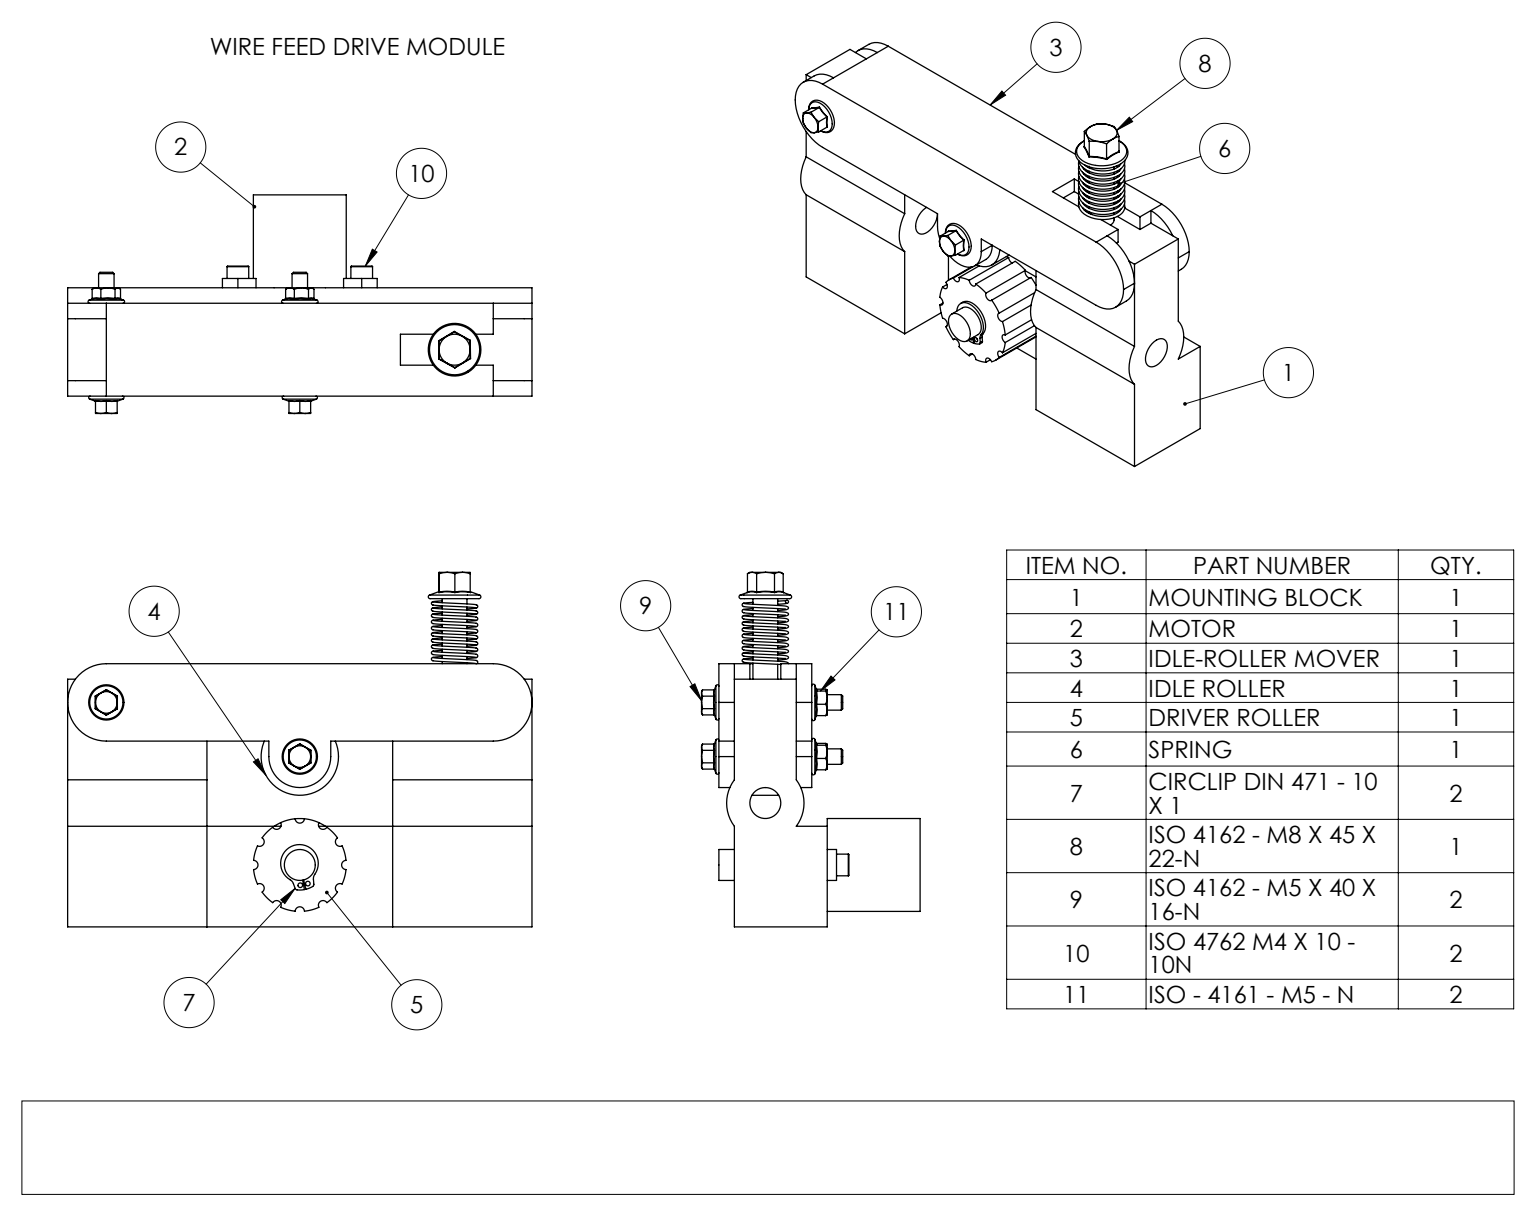
ISO-10303-21;
HEADER;
FILE_DESCRIPTION (('STEP AP214'),
    '1' );
FILE_NAME ('MAS-183',
    '2026-10-25T07:12:54',
    ( '' ),
    ( '' ),
    'SwSTEP 2.0',
    'SolidWorks 2026',
    '' );
FILE_SCHEMA (( 'AUTOMOTIVE_DESIGN' ));
ENDSEC;

DATA;
#1 = CARTESIAN_POINT ( 'NONE',  ( 44.30067958973594955, 46.10051614449766078, -1.875703265242155693 ) ) ;
#2 = CARTESIAN_POINT ( 'NONE',  ( 43.33558569842706021, 59.90051614449766504, 2.141517661632167169 ) ) ;
#3 = CARTESIAN_POINT ( 'NONE',  ( 56.81924384183011512, 48.19948385550240744, 4.924951120819313743 ) ) ;
#4 = DIRECTION ( 'NONE',  ( 0.4999999999999977796, 0.8660254037844398178, 0.000000000000000000 ) ) ;
#5 = CARTESIAN_POINT ( 'NONE',  ( 49.97728705011495265, 53.50051614449767357, 8.000000000000001776 ) ) ;
#6 =( REPRESENTATION_RELATIONSHIP ('NONE','NONE', #5328, #4503 ) REPRESENTATION_RELATIONSHIP_WITH_TRANSFORMATION ( #11054 )SHAPE_REPRESENTATION_RELATIONSHIP( ) );
#8 = EDGE_CURVE ( 'NONE', #8677, #8586, #7240, .T. ) ;
#7 = EDGE_LOOP ( 'NONE', ( #12409, #2488, #778, #882 ) ) ;
#9 = STYLED_ITEM ( 'NONE', ( #1512 ), #12751 ) ;
#10 = ORIENTED_EDGE ( 'NONE', *, *, #6895, .T. ) ;
#11 = ORIENTED_EDGE ( 'NONE', *, *, #3487, .F. ) ;
#12 = AXIS2_PLACEMENT_3D ( 'NONE', #12108, #3741, #674 ) ;
#13 = CARTESIAN_POINT ( 'NONE',  ( 62.49999999999998579, 40.00000000000001421, 0.000000000000000000 ) ) ;
#14 = SURFACE_STYLE_FILL_AREA ( #11634 ) ;
#15 = CARTESIAN_POINT ( 'NONE',  ( 2.449293598294706513E-15, -35.00000000000000000, 9.000000000000000000 ) ) ;
#16 = CARTESIAN_POINT ( 'NONE',  ( -2.100000000000000089, 2.571758278209441957E-16, -4.694516984716113228 ) ) ;
#17 = CARTESIAN_POINT ( 'NONE',  ( 44.28664221472220675, 51.09948385550240602, -1.832500667257165317 ) ) ;
#18 = CARTESIAN_POINT ( 'NONE',  ( 44.03140696652193498, 63.19948385550240744, -4.306917132069424170 ) ) ;
#19 = ADVANCED_FACE ( 'NONE', ( #12392 ), #1035, .T. ) ;
#20 = CARTESIAN_POINT ( 'NONE',  ( 47.70284917648459100, 63.60051614449766078, 6.992620115222796251 ) ) ;
#21 = AXIS2_PLACEMENT_3D ( 'NONE', #13643, #10746, #12742 ) ;
#22 = EDGE_CURVE ( 'NONE', #9726, #725, #6704, .T. ) ;
#23 = DIRECTION ( 'NONE',  ( 1.000000000000000000, 3.469446951953615668E-16, -0.000000000000000000 ) ) ;
#24 = DIRECTION ( 'NONE',  ( -1.000000000000000000, 9.251858538542972814E-17, -0.000000000000000000 ) ) ;
#25 = DIRECTION ( 'NONE',  ( -0.000000000000000000, -0.000000000000000000, 1.000000000000000000 ) ) ;
#26 = CARTESIAN_POINT ( 'NONE',  ( 57.36023556966787851, 57.00051614449766646, 0.02388180880515038476 ) ) ;
#27 = CARTESIAN_POINT ( 'NONE',  ( 55.69932041026404335, 55.89948385550241028, -1.875703265242203432 ) ) ;
#28 = FACE_OUTER_BOUND ( 'NONE', #7057, .T. ) ;
#29 = ORIENTED_EDGE ( 'NONE', *, *, #7296, .F. ) ;
#30 = CARTESIAN_POINT ( 'NONE',  ( 22.14999999999999858, -20.00000000000000000, -23.00000000000000000 ) ) ;
#31 = ORIENTED_EDGE ( 'NONE', *, *, #5701, .T. ) ;
#32 = FACE_OUTER_BOUND ( 'NONE', #8639, .T. ) ;
#33 = AXIS2_PLACEMENT_3D ( 'NONE', #4037, #13487, #9223 ) ;
#34 = PRODUCT_DEFINITION_SHAPE ( 'NONE', 'NONE',  #13671 ) ;
#35 = VECTOR ( 'NONE', #3248, 1000.000000000000000 ) ;
#36 = FACE_OUTER_BOUND ( 'NONE', #13516, .T. ) ;
#37 = DIRECTION ( 'NONE',  ( 1.000000000000000000, 0.000000000000000000, 0.000000000000000000 ) ) ;
#38 = DIRECTION ( 'NONE',  ( 0.000000000000000000, 0.000000000000000000, 1.000000000000000000 ) ) ;
#39 = CARTESIAN_POINT ( 'NONE',  ( 54.13287192849676188, 50.29948385550240175, 5.649768623646098220 ) ) ;
#40 = EDGE_CURVE ( 'NONE', #11408, #11811, #8258, .T. ) ;
#41 = CARTESIAN_POINT ( 'NONE',  ( -1.360585162435467455, 4.061296242128285883, -3.505054077164959203 ) ) ;
#42 = CARTESIAN_POINT ( 'NONE',  ( 51.97223112728249816, 54.60051614449766788, -5.992620115222793586 ) ) ;
#43 = CARTESIAN_POINT ( 'NONE',  ( 6.367873360227555679, -2.886751345948119774, 4.999999999999999112 ) ) ;
#44 = CARTESIAN_POINT ( 'NONE',  ( 49.97728705011488159, 65.49948385550240459, -7.000000000000000888 ) ) ;
#45 = CARTESIAN_POINT ( 'NONE',  ( 56.65037692655918988, 61.89948385550241028, -2.184720259617163762 ) ) ;
#46 = CARTESIAN_POINT ( 'NONE',  ( 56.65037692655918988, 57.89948385550240317, -2.184720259617163762 ) ) ;
#47 = VECTOR ( 'NONE', #619, 1000.000000000000000 ) ;
#48 = TOROIDAL_SURFACE ( 'NONE', #12842, 7.900000000000002132, 0.5999999999999979794 ) ;
#49 = VECTOR ( 'NONE', #8618, 1000.000000000000000 ) ;
#50 = ORIENTED_EDGE ( 'NONE', *, *, #11088, .F. ) ;
#51 = ORIENTED_EDGE ( 'NONE', *, *, #11790, .T. ) ;
#52 = EDGE_CURVE ( 'NONE', #12021, #8324, #11821, .T. ) ;
#53 = PLANE ( 'NONE',  #5492 ) ;
#54 = CARTESIAN_POINT ( 'NONE',  ( 3.861362476283255685, 2.629030857715988656, -3.671615880910370500 ) ) ;
#55 = CARTESIAN_POINT ( 'NONE',  ( 4.055492966679659084, -3.795017426214758682, 0.5629142681442622642 ) ) ;
#56 = VECTOR ( 'NONE', #10401, 1000.000000000000114 ) ;
#57 = CARTESIAN_POINT ( 'NONE',  ( 2.000000000000000000, 0.000000000000000000, 0.000000000000000000 ) ) ;
#58 = CARTESIAN_POINT ( 'NONE',  ( 56.66441430157296821, 48.09948385550240602, 2.141517661632100111 ) ) ;
#59 = AXIS2_PLACEMENT_3D ( 'NONE', #3052, #893, #11418 ) ;
#60 = CARTESIAN_POINT ( 'NONE',  ( 56.66441430157294690, 48.90051614449766504, -2.141517661632166281 ) ) ;
#61 = DIRECTION ( 'NONE',  ( -1.000000000000000000, 0.000000000000000000, 0.000000000000000000 ) ) ;
#62 = CARTESIAN_POINT ( 'NONE',  ( 47.42335538002188144, 62.59948385550238470, 8.007379884777233059 ) ) ;
#63 =( LENGTH_UNIT ( ) NAMED_UNIT ( * ) SI_UNIT ( .MILLI., .METRE. ) );
#64 = CARTESIAN_POINT ( 'NONE',  ( 56.79116909180255135, 53.79948385550241596, -4.963592699179005585 ) ) ;
#65 = VERTEX_POINT ( 'NONE', #4105 ) ;
#66 = CIRCLE ( 'NONE', #7586, 1.500000000000001110 ) ;
#67 = EDGE_LOOP ( 'NONE', ( #6510, #1768, #3467, #950 ) ) ;
#68 = LINE ( 'NONE', #4288, #2309 ) ;
#69 = CARTESIAN_POINT ( 'NONE',  ( 6.207671477327291853, -3.321994320370684317, 4.246137054662720622 ) ) ;
#70=STYLED_ITEM('',(#13712),#1029);
#71 = FACE_OUTER_BOUND ( 'NONE', #6413, .T. ) ;
#72 = CARTESIAN_POINT ( 'NONE',  ( 55.08986747509849380, 47.20051614449766220, 3.727524721679155384 ) ) ;
#73 = CARTESIAN_POINT ( 'NONE',  ( 52.25172492374528588, 57.40051614449765793, 7.007379884777204637 ) ) ;
#74 = CARTESIAN_POINT ( 'NONE',  ( 52.57664461997811856, 45.59948385550240602, -8.007379884777229506 ) ) ;
#75 = CARTESIAN_POINT ( 'NONE',  ( 4.052424581287595196, 3.786734753434853662, 0.5771415817955924954 ) ) ;
#76 = CARTESIAN_POINT ( 'NONE',  ( 58.41169779390614281, 55.00051614449766646, 0.02388180880515032231 ) ) ;
#77 = ORIENTED_EDGE ( 'NONE', *, *, #7381, .F. ) ;
#78 = ORIENTED_EDGE ( 'NONE', *, *, #4870, .T. ) ;
#79 = ORIENTED_EDGE ( 'NONE', *, *, #8111, .F. ) ;
#80 = CYLINDRICAL_SURFACE ( 'NONE', #13518, 1.500000000000001332 ) ;
#81 = EDGE_CURVE ( 'NONE', #6144, #12887, #9290, .T. ) ;
#83 = CIRCLE ( 'NONE', #7166, 4.999999999999999112 ) ;
#82 = PLANE ( 'NONE',  #5621 ) ;
#84 = CARTESIAN_POINT ( 'NONE',  ( 5.599999999999999645, 4.041451884327382338, 0.000000000000000000 ) ) ;
#85 = DIRECTION ( 'NONE',  ( 1.000000000000000000, -0.000000000000000000, 0.000000000000000000 ) ) ;
#86 = CARTESIAN_POINT ( 'NONE',  ( 48.02776887271745210, 49.39948385550241028, -5.992620115222778487 ) ) ;
#87 = CARTESIAN_POINT ( 'NONE',  ( 4.050880675075949178, 1.379097446046194220, 3.567934390854430760 ) ) ;
#88 = CARTESIAN_POINT ( 'NONE',  ( 54.72065718078918906, 48.70051614449766930, -6.458785618021089192 ) ) ;
#89 = CARTESIAN_POINT ( 'NONE',  ( 4.000000000000000888, 1.539600717838996990, -3.300726591567079815 ) ) ;
#90 = CARTESIAN_POINT ( 'NONE',  ( 0.08165819712376973238, 4.939961795957293234, 1.443735181952769064 ) ) ;
#91 = CARTESIAN_POINT ( 'NONE',  ( 47.74827507625469281, 54.40051614449766504, -7.007379884777203749 ) ) ;
#92 = CARTESIAN_POINT ( 'NONE',  ( 50.02271294988511841, 56.49948385550240459, 6.000000000000000888 ) ) ;
#93 = CARTESIAN_POINT ( 'NONE',  ( 2.000000000000000000, -6.429618962271402616, -1.000000000000000000 ) ) ;
#94 = ADVANCED_FACE ( 'NONE', ( #8455 ), #6331, .F. ) ;
#95 = CIRCLE ( 'NONE', #11121, 2.649999999999988365 ) ;
#96 = ORIENTED_EDGE ( 'NONE', *, *, #7070, .F. ) ;
#97 = ADVANCED_FACE ( 'NONE', ( #1883, #8329, #2085 ), #7362, .T. ) ;
#98 = DIRECTION ( 'NONE',  ( 0.000000000000000000, -1.000000000000000000, 0.000000000000000000 ) ) ;
#99 = EDGE_CURVE ( 'NONE', #9288, #2470, #13475, .T. ) ;
#100 = AXIS2_PLACEMENT_3D ( 'NONE', #7790, #12001, #438 ) ;
#101 = ORIENTED_EDGE ( 'NONE', *, *, #5437, .F. ) ;
#102 = DIRECTION ( 'NONE',  ( 1.000000000000000000, 0.000000000000000000, 0.000000000000000000 ) ) ;
#103 = EDGE_CURVE ( 'NONE', #12840, #3906, #7426, .T. ) ;
#104 = DIRECTION ( 'NONE',  ( -9.710251638871371392E-17, -5.969973981896233748E-17, -1.000000000000000000 ) ) ;
#105 = CARTESIAN_POINT ( 'NONE',  ( 4.093692494532774617, 2.021783646005766322, -3.501831996793843160 ) ) ;
#106 = SURFACE_STYLE_USAGE ( .BOTH. , #7508 ) ;
#107 = CARTESIAN_POINT ( 'NONE',  ( 54.13287192849676188, 52.29948385550240886, 5.649768623646098220 ) ) ;
#108 = AXIS2_PLACEMENT_3D ( 'NONE', #135, #10772, #2266 ) ;
#109 = CARTESIAN_POINT ( 'NONE',  ( 53.50833635130544508, 51.30051614449765651, 4.867452303228181343 ) ) ;
#110 = CARTESIAN_POINT ( 'NONE',  ( 2.385244779468109755E-15, -20.00000000000000000, -9.999999999999994671 ) ) ;
#111 = LINE ( 'NONE', #5314, #1494 ) ;
#112 = CARTESIAN_POINT ( 'NONE',  ( 6.466260427357665819, -5.808561367196025671, 1.503437176544561004E-15 ) ) ;
#113 = CARTESIAN_POINT ( 'NONE',  ( 47.74827507625478518, 60.59948385550239891, 7.007379884777227730 ) ) ;
#114 = CARTESIAN_POINT ( 'NONE',  ( -0.2500000000000000000, -8.096141056083446585, -1.000000000000000000 ) ) ;
#115 = ORIENTED_EDGE ( 'NONE', *, *, #9892, .T. ) ;
#116 = EDGE_LOOP ( 'NONE', ( #1810, #12426, #10336 ) ) ;
#117 = AXIS2_PLACEMENT_3D ( 'NONE', #12874, #6605, #168 ) ;
#118 = ORIENTED_EDGE ( 'NONE', *, *, #4262, .T. ) ;
#119 = CARTESIAN_POINT ( 'NONE',  ( -1.287237434361707233, -3.875615274277397937, -3.430618716626816500 ) ) ;
#120 = ADVANCED_FACE ( 'NONE', ( #5352 ), #80, .F. ) ;
#121 = B_SPLINE_CURVE_WITH_KNOTS ( 'NONE', 3,
 ( #11045, #8921, #1705, #7048, #10078, #9050 ),
 .UNSPECIFIED., .F., .F.,
 ( 4, 2, 4 ),
 ( 0.000000000000000000, 0.002086519881787260184, 0.004173039763574520368 ),
 .UNSPECIFIED. ) ;
#122 = CARTESIAN_POINT ( 'NONE',  ( 0.000000000000000000, 0.000000000000000000, 0.000000000000000000 ) ) ;
#123 = CARTESIAN_POINT ( 'NONE',  ( -3.355112389629170799, 2.681727112203152963, -0.2256878752776689534 ) ) ;
#124 = CARTESIAN_POINT ( 'NONE',  ( 4.024499207728657879, 2.323545700935571556, -3.572172305156506411 ) ) ;
#125 = CARTESIAN_POINT ( 'NONE',  ( 56.65037692655918988, 49.89948385550240317, -2.184720259617163762 ) ) ;
#126 = CARTESIAN_POINT ( 'NONE',  ( 56.65037692655921120, 45.10051614449766078, 2.184720259617097593 ) ) ;
#127 = DIRECTION ( 'NONE',  ( 0.000000000000000000, 0.000000000000000000, 1.000000000000000000 ) ) ;
#128 = CARTESIAN_POINT ( 'NONE',  ( 50.02271294988512551, 48.49948385550240459, 7.000000000000000888 ) ) ;
#129 = CYLINDRICAL_SURFACE ( 'NONE', #612, 2.500000000000000444 ) ;
#130 = CARTESIAN_POINT ( 'NONE',  ( 56.81924384183011512, 54.19948385550241454, 4.924951120819313743 ) ) ;
#131 = ORIENTED_EDGE ( 'NONE', *, *, #11542, .F. ) ;
#132 = EDGE_CURVE ( 'NONE', #594, #13026, #10926, .T. ) ;
#133 = EDGE_LOOP ( 'NONE', ( #295, #3127 ) ) ;
#134 = EDGE_CURVE ( 'NONE', #822, #8082, #1591, .T. ) ;
#135 = CARTESIAN_POINT ( 'NONE',  ( 1.267864665261691752E-11, -20.00000000000000000, 9.999999999999998224 ) ) ;
#136 = AXIS2_PLACEMENT_3D ( 'NONE', #12197, #10046, #9019 ) ;
#137 = CARTESIAN_POINT ( 'NONE',  ( 50.00000000000000000, 40.00000000000000000, 0.000000000000000000 ) ) ;
#138 = CARTESIAN_POINT ( 'NONE',  ( 46.45491332379576477, 49.70051614449766220, 4.840751629271188961 ) ) ;
#139 = CARTESIAN_POINT ( 'NONE',  ( 47.74827507625470702, 60.40051614449766504, -7.007379884777204637 ) ) ;
#140 = CARTESIAN_POINT ( 'NONE',  ( 47.37792948025170858, 63.60051614449764656, 7.992620115222797139 ) ) ;
#141 = CARTESIAN_POINT ( 'NONE',  ( -75.00000000000001421, -5.000000000000025757, 6.123233995736775157E-16 ) ) ;
#142 = B_SPLINE_CURVE_WITH_KNOTS ( 'NONE', 3,
 ( #2843, #11275, #8032, #7064, #8173 ),
 .UNSPECIFIED., .F., .F.,
 ( 4, 1, 4 ),
 ( 0.000000000000000000, 0.002020725942163692675, 0.004041451884327385349 ),
 .UNSPECIFIED. ) ;
#143 = CARTESIAN_POINT ( 'NONE',  ( 47.37792948025170858, 53.60051614449765367, 7.992620115222797139 ) ) ;
#144 = B_SPLINE_CURVE_WITH_KNOTS ( 'NONE', 3,
 ( #13141, #2570, #7772, #10101, #12115, #12051, #4654, #11983, #6798, #4863, #3822, #8039 ),
 .UNSPECIFIED., .F., .F.,
 ( 4, 2, 2, 2, 2, 4 ),
 ( 0.01755862241325779893, 0.01812962329865995884, 0.01870062418406211874, 0.01984262595486643854, 0.02098462772567075835, 0.02212662949647507815 ),
 .UNSPECIFIED. ) ;
#145 = PRODUCT_DEFINITION_SHAPE ( 'NONE', 'NONE',  #13669 ) ;
#146 = ORIENTED_EDGE ( 'NONE', *, *, #5916, .F. ) ;
#147 = CONICAL_SURFACE ( 'NONE', #11179, 8.105212085995399107, 1.221730476396037490 ) ;
#148 = ORIENTED_EDGE ( 'NONE', *, *, #10663, .F. ) ;
#149 = ORIENTED_EDGE ( 'NONE', *, *, #1777, .T. ) ;
#150 = ORIENTED_EDGE ( 'NONE', *, *, #2542, .F. ) ;
#151 = DIRECTION ( 'NONE',  ( -0.5000000000000041078, 0.8660254037844362651, 0.000000000000000000 ) ) ;
#152 = FACE_OUTER_BOUND ( 'NONE', #7758, .T. ) ;
#153 = FACE_OUTER_BOUND ( 'NONE', #3940, .T. ) ;
#154 = FACE_OUTER_BOUND ( 'NONE', #10455, .T. ) ;
#155 = CARTESIAN_POINT ( 'NONE',  ( 55.71335778527780747, 50.09948385550240602, 1.832500667257165983 ) ) ;
#156 = CARTESIAN_POINT ( 'NONE',  ( 47.74827507625477807, 64.59948385550239891, 7.007379884777229506 ) ) ;
#157 = ADVANCED_FACE ( 'NONE', ( #8524 ), #11972, .T. ) ;
#158 = CARTESIAN_POINT ( 'NONE',  ( 45.90387839640208512, 64.30051614449766362, -5.676469297603124353 ) ) ;
#159 = DIRECTION ( 'NONE',  ( -1.000000000000000000, 0.000000000000000000, 0.000000000000000000 ) ) ;
#160 = CARTESIAN_POINT ( 'NONE',  ( 4.000000000000003553, 4.286263797015736595E-16, -3.500000000000000000 ) ) ;
#161 = CARTESIAN_POINT ( 'NONE',  ( 45.90387839640208512, 54.30051614449765651, -5.676469297603124353 ) ) ;
#162 = CARTESIAN_POINT ( 'NONE',  ( 55.11794222512601493, 60.19948385550240744, 3.688883143319541702 ) ) ;
#163 = ADVANCED_FACE ( 'NONE', ( #12857 ), #1236, .F. ) ;
#164 = ORIENTED_EDGE ( 'NONE', *, *, #12600, .T. ) ;
#165 = CARTESIAN_POINT ( 'NONE',  ( -9.999999999999996447, 0.000000000000000000, 9.999999999999998224 ) ) ;
#166 = ORIENTED_EDGE ( 'NONE', *, *, #5950, .F. ) ;
#167 = CARTESIAN_POINT ( 'NONE',  ( -75.00000000000001421, -2.602085213965211904E-14, 0.000000000000000000 ) ) ;
#168 = DIRECTION ( 'NONE',  ( 0.000000000000000000, 0.000000000000000000, 1.000000000000000000 ) ) ;
#169 = CARTESIAN_POINT ( 'NONE',  ( -4.000000000000000000, -0.7890432684750890990, -0.04868663549882315533 ) ) ;
#170 = CARTESIAN_POINT ( 'NONE',  ( 45.86712807150323812, 53.29948385550240886, -5.649768623646098220 ) ) ;
#171 = PLANE ( 'NONE',  #421 ) ;
#172 = CARTESIAN_POINT ( 'NONE',  ( 48.02776887271750184, 51.60051614449766788, 5.992620115222795363 ) ) ;
#173 = DIRECTION ( 'NONE',  ( 1.000000000000000000, 0.000000000000000000, 0.000000000000000000 ) ) ;
#174 = FACE_OUTER_BOUND ( 'NONE', #12287, .T. ) ;
#175 = CARTESIAN_POINT ( 'NONE',  ( 6.527192678185836705, -5.883244248022288403, -1.193258867985458992E-13 ) ) ;
#176 = CARTESIAN_POINT ( 'NONE',  ( 55.94051828345050836, 57.79948385550238754, -4.345558710429104465 ) ) ;
#177 = FACE_OUTER_BOUND ( 'NONE', #6171, .T. ) ;
#178 = VERTEX_POINT ( 'NONE', #7689 ) ;
#179 = ORIENTED_EDGE ( 'NONE', *, *, #103, .F. ) ;
#180 = SHAPE_REPRESENTATION ( 'hex flange nut gradea_iso_ISO - 4161 - M5 - N', ( #430 ), #9487 ) ;
#181 = ORIENTED_EDGE ( 'NONE', *, *, #4567, .T. ) ;
#182 = FACE_OUTER_BOUND ( 'NONE', #2923, .T. ) ;
#183 = FACE_OUTER_BOUND ( 'NONE', #3328, .T. ) ;
#184 = CARTESIAN_POINT ( 'NONE',  ( 4.033901012035946643, -3.740908793664254883, 0.5205559028926849408 ) ) ;
#185 =( NAMED_UNIT ( * ) SI_UNIT ( $, .STERADIAN. ) SOLID_ANGLE_UNIT ( ) );
#186 = FACE_OUTER_BOUND ( 'NONE', #2806, .T. ) ;
#187 = CARTESIAN_POINT ( 'NONE',  ( 45.86712807150323812, 51.29948385550240175, -5.649768623646098220 ) ) ;
#188 = CARTESIAN_POINT ( 'NONE',  ( 47.74827507625469281, 56.40051614449766504, -7.007379884777203749 ) ) ;
#189 = CIRCLE ( 'NONE', #9683, 1.610000000000000098 ) ;
#190 = FACE_OUTER_BOUND ( 'NONE', #6460, .T. ) ;
#191 = CARTESIAN_POINT ( 'NONE',  ( 54.72065718078924590, 64.29948385550240175, 6.458785618021043895 ) ) ;
#192 = ADVANCED_FACE ( 'NONE', ( #1373 ), #9888, .F. ) ;
#193 = CYLINDRICAL_SURFACE ( 'NONE', #11066, 15.00000000000000000 ) ;
#194 = EDGE_CURVE ( 'NONE', #11144, #6641, #2280, .T. ) ;
#195 = B_SPLINE_CURVE_WITH_KNOTS ( 'NONE', 3,
 ( #11262, #10080, #4985, #5816, #13250 ),
 .UNSPECIFIED., .F., .F.,
 ( 4, 1, 4 ),
 ( 0.000000000000000000, 0.002886751345948130286, 0.005773502691896260572 ),
 .UNSPECIFIED. ) ;
#196 = CARTESIAN_POINT ( 'NONE',  ( 45.27934281921075410, 57.29948385550240175, -6.458785618021043895 ) ) ;
#197 = EDGE_CURVE ( 'NONE', #1117, #3434, #12820, .T. ) ;
#198 = ORIENTED_EDGE ( 'NONE', *, *, #8722, .T. ) ;
#199 = ORIENTED_EDGE ( 'NONE', *, *, #13522, .F. ) ;
#200 = CARTESIAN_POINT ( 'NONE',  ( 32.49999999999998579, 40.00000000000001421, -4.999999999999996447 ) ) ;
#201 = CIRCLE ( 'NONE', #9264, 1.500000000000000222 ) ;
#202 = CARTESIAN_POINT ( 'NONE',  ( -14.99999999999999822, -19.99999999999999645, -23.00000000000000000 ) ) ;
#203 = CARTESIAN_POINT ( 'NONE',  ( 43.69122665457040000, 56.00051614449765935, -0.02388180880515696977 ) ) ;
#204 = CARTESIAN_POINT ( 'NONE',  ( 8.673617379884035472E-16, 4.618802153517012954, 0.000000000000000000 ) ) ;
#205 = PRESENTATION_LAYER_ASSIGNMENT (  '', '', ( #8165 ) ) ;
#206 = CARTESIAN_POINT ( 'NONE',  ( 54.68390685589033495, 45.69948385550240033, -6.485486291978119766 ) ) ;
#207 = VECTOR ( 'NONE', #526, 1000.000000000000000 ) ;
#208 = CARTESIAN_POINT ( 'NONE',  ( 2.449293598294706513E-15, -20.00000000000000000, -9.000000000000000000 ) ) ;
#209 = CARTESIAN_POINT ( 'NONE',  ( 45.27934281921082516, 53.70051614449766220, 6.458785618021089192 ) ) ;
#210 = ORIENTED_EDGE ( 'NONE', *, *, #1266, .T. ) ;
#211 = ORIENTED_EDGE ( 'NONE', *, *, #8650, .F. ) ;
#212 = ORIENTED_EDGE ( 'NONE', *, *, #12682, .T. ) ;
#213 = ORIENTED_EDGE ( 'NONE', *, *, #10321, .T. ) ;
#214 = AXIS2_PLACEMENT_3D ( 'NONE', #5780, #4595, #6805 ) ;
#215 = DIRECTION ( 'NONE',  ( 0.000000000000000000, 0.000000000000000000, 1.000000000000000000 ) ) ;
#216 = EDGE_CURVE ( 'NONE', #11745, #13576, #7487, .T. ) ;
#218 = CIRCLE ( 'NONE', #6639, 5.000000000000000000 ) ;
#217 = DIRECTION ( 'NONE',  ( -0.000000000000000000, -0.000000000000000000, -1.000000000000000000 ) ) ;
#219 = FACE_BOUND ( 'NONE', #1402, .T. ) ;
#220 = CARTESIAN_POINT ( 'NONE',  ( -74.99999999999997158, 20.00000000000001421, 15.00000000000000000 ) ) ;
#221 = CYLINDRICAL_SURFACE ( 'NONE', #6994, 2.000000000000000888 ) ;
#222 = CARTESIAN_POINT ( 'NONE',  ( 51.97223112728254790, 50.39948385550241738, 5.992620115222778487 ) ) ;
#223 = CARTESIAN_POINT ( 'NONE',  ( 43.33558569842703179, 63.09948385550240602, -2.141517661632099223 ) ) ;
#224 = CARTESIAN_POINT ( 'NONE',  ( 41.58830220609386430, 48.00051614449766646, -0.02388180880514929535 ) ) ;
#225 = CARTESIAN_POINT ( 'NONE',  ( -0.1481481481481481122, -4.797713218419819903, -1.000000000000000000 ) ) ;
#226 = CARTESIAN_POINT ( 'NONE',  ( -4.000000000000000000, -2.309401076758512694, -5.000000000000000000 ) ) ;
#227 = EDGE_CURVE ( 'NONE', #4104, #6571, #11764, .T. ) ;
#228 = CARTESIAN_POINT ( 'NONE',  ( 56.65037692655921120, 57.10051614449766078, 2.184720259617097593 ) ) ;
#229 =( GEOMETRIC_REPRESENTATION_CONTEXT ( 3 ) GLOBAL_UNCERTAINTY_ASSIGNED_CONTEXT ( ( #8327 ) ) GLOBAL_UNIT_ASSIGNED_CONTEXT ( ( #1931, #1865, #3739 ) ) REPRESENTATION_CONTEXT ( 'NONE', 'WORKASPACE' ) );
#230 = CARTESIAN_POINT ( 'NONE',  ( 55.71335778527780747, 58.09948385550241312, 1.832500667257165983 ) ) ;
#231 = VECTOR ( 'NONE', #11750, 1000.000000000000000 ) ;
#232 = ORIENTED_EDGE ( 'NONE', *, *, #13179, .F. ) ;
#233 = PLANE ( 'NONE',  #5515 ) ;
#234 = ORIENTED_EDGE ( 'NONE', *, *, #2081, .F. ) ;
#235 = CARTESIAN_POINT ( 'NONE',  ( 6.527192678185834041, 2.941622124011172623, 5.095038975455953079 ) ) ;
#236 = FACE_OUTER_BOUND ( 'NONE', #5614, .T. ) ;
#237 = CARTESIAN_POINT ( 'NONE',  ( 4.050823680195223098, 2.400527758044901372, 2.978030508226146900 ) ) ;
#238 = CARTESIAN_POINT ( 'NONE',  ( 45.90387839640214196, 48.69948385550240744, 5.676469297603166098 ) ) ;
#239 = CARTESIAN_POINT ( 'NONE',  ( 2.449293598294706513E-15, -20.00000000000000000, 9.000000000000000000 ) ) ;
#240 = CARTESIAN_POINT ( 'NONE',  ( 43.69122665457040000, 60.00051614449765935, -0.02388180880515696977 ) ) ;
#241 = CARTESIAN_POINT ( 'NONE',  ( -30.00000000000000000, 7.499999999999991118, 10.00000000000000000 ) ) ;
#242 = DIRECTION ( 'NONE',  ( 1.000000000000000000, 0.000000000000000000, 0.000000000000000000 ) ) ;
#243 = CARTESIAN_POINT ( 'NONE',  ( 52.29715082351547295, 60.39948385550239607, 6.992620115222774047 ) ) ;
#244 = DIRECTION ( 'NONE',  ( 0.000000000000000000, -0.000000000000000000, 1.000000000000000000 ) ) ;
#245 = VERTEX_POINT ( 'NONE', #4504 ) ;
#246 = VECTOR ( 'NONE', #11169, 1000.000000000000000 ) ;
#247 = ORIENTED_EDGE ( 'NONE', *, *, #4058, .T. ) ;
#248 = CARTESIAN_POINT ( 'NONE',  ( 0.1410422978106145031, -4.700232962125109104, -3.687027686973628704 ) ) ;
#249 = DIRECTION ( 'NONE',  ( 0.000000000000000000, 0.000000000000000000, 1.000000000000000000 ) ) ;
#250 = DIRECTION ( 'NONE',  ( -0.7581610723493046322, -0.6520673188974834833, 1.125475972357111981E-16 ) ) ;
#251 = CARTESIAN_POINT ( 'NONE',  ( 20.00000000000000000, -20.00000000000000000, -12.00000000000000000 ) ) ;
#252 = FACE_BOUND ( 'NONE', #2068, .T. ) ;
#253 = CARTESIAN_POINT ( 'NONE',  ( 43.34962307344081012, 54.89948385550240317, 2.184720259617164650 ) ) ;
#254 = CARTESIAN_POINT ( 'NONE',  ( 56.65037692655921120, 55.10051614449766078, 2.184720259617097593 ) ) ;
#255 = CARTESIAN_POINT ( 'NONE',  ( 75.00000000000001421, 2.602085213965211904E-14, 0.000000000000000000 ) ) ;
#256 = AXIS2_PLACEMENT_3D ( 'NONE', #2457, #12077, #2596 ) ;
#257 = CARTESIAN_POINT ( 'NONE',  ( 43.33558569842703179, 49.09948385550240602, -2.141517661632099223 ) ) ;
#258 =( BOUNDED_SURFACE ( )  B_SPLINE_SURFACE ( 3, 2, ( 
 ( #4456, #8885, #3626 ),
 ( #7848, #4733, #425 ),
 ( #12875, #2579, #6804 ),
 ( #11009, #4594, #5571 ),
 ( #1531, #5776, #3689 ),
 ( #9780, #6677, #7912 ) ),
 .UNSPECIFIED., .F., .F., .F. ) 
 B_SPLINE_SURFACE_WITH_KNOTS ( ( 4, 2, 4 ),
 ( 3, 3 ),
 ( 0.01651999345535506980, 0.01858032176739836394, 0.02064065007944165808 ),
 ( 0.000000000000000000, 1.000000000000000000 ),
 .UNSPECIFIED. ) 
 GEOMETRIC_REPRESENTATION_ITEM ( )  RATIONAL_B_SPLINE_SURFACE ( (
 ( 1.000000000000000000, 0.8047781103519393575, 1.000000000000000000),
 ( 1.000000000000000000, 0.8123785825603968558, 1.000000000000000000),
 ( 1.000000000000000000, 0.8190671539788806355, 1.000000000000000000),
 ( 1.000000000000000000, 0.8192352254834333047, 1.000000000000000000),
 ( 1.000000000000000000, 0.8126129677212012847, 1.000000000000000000),
 ( 1.000000000000000000, 0.8047712537969730073, 1.000000000000000000) ) ) 
 REPRESENTATION_ITEM ( '' )  SURFACE ( )  );
#259 = CARTESIAN_POINT ( 'NONE',  ( 47.42335538002188144, 62.59948385550238470, 8.007379884777233059 ) ) ;
#260 = EDGE_CURVE ( 'NONE', #13554, #4523, #9345, .T. ) ;
#261 = ORIENTED_EDGE ( 'NONE', *, *, #227, .F. ) ;
#262 = AXIS2_PLACEMENT_3D ( 'NONE', #4018, #5829, #10026 ) ;
#263 = ORIENTED_EDGE ( 'NONE', *, *, #4115, .F. ) ;
#264 = ADVANCED_FACE ( 'NONE', ( #3266 ), #5618, .F. ) ;
#265 = CARTESIAN_POINT ( 'NONE',  ( 2.449293598294706513E-15, -20.00000000000000000, 9.000000000000000000 ) ) ;
#266 = ADVANCED_FACE ( 'NONE', ( #8732 ), #10661, .F. ) ;
#267 = EDGE_CURVE ( 'NONE', #10003, #9221, #8792, .T. ) ;
#268 = DIRECTION ( 'NONE',  ( 0.3420201433256622736, 0.000000000000000000, -0.9396926207859106484 ) ) ;
#269 = CARTESIAN_POINT ( 'NONE',  ( 46.45491332379576477, 51.70051614449765509, 4.840751629271188961 ) ) ;
#270 = CARTESIAN_POINT ( 'NONE',  ( -3.333333333333335258, 2.694301256218251783, -3.300726591567079815 ) ) ;
#271 = CARTESIAN_POINT ( 'NONE',  ( 52.57664461997811856, 51.59948385550240602, -8.007379884777229506 ) ) ;
#272 = EDGE_CURVE ( 'NONE', #12293, #940, #9194, .T. ) ;
#273 = CARTESIAN_POINT ( 'NONE',  ( 55.96859303347804371, 56.19948385550241454, 4.306917132069425946 ) ) ;
#274 = CARTESIAN_POINT ( 'NONE',  ( 3.972066048304770725, 3.435565134476467275, 1.180968096049824556 ) ) ;
#275 = CARTESIAN_POINT ( 'NONE',  ( 47.42335538002180328, 58.40051614449765793, -8.007379884777206414 ) ) ;
#276 = AXIS2_PLACEMENT_3D ( 'NONE', #9355, #962, #6117 ) ;
#277 = ORIENTED_EDGE ( 'NONE', *, *, #8722, .F. ) ;
#278 = VERTEX_POINT ( 'NONE', #10857 ) ;
#279 = ORIENTED_EDGE ( 'NONE', *, *, #2210, .T. ) ;
#280 = ORIENTED_EDGE ( 'NONE', *, *, #5001, .F. ) ;
#281 = EDGE_CURVE ( 'NONE', #5149, #3301, #7761, .T. ) ;
#282 = CARTESIAN_POINT ( 'NONE',  ( -3.679171394226034675, -2.494631558665844739, -0.3503314178412558211 ) ) ;
#283 = CYLINDRICAL_SURFACE ( 'NONE', #7915, 5.000000000000000888 ) ;
#284 = EDGE_CURVE ( 'NONE', #3263, #6584, #5155, .T. ) ;
#285 = CARTESIAN_POINT ( 'NONE',  ( 0.4465819873852002742, 2.886751345948125547, 4.999999999999999112 ) ) ;
#286 = CARTESIAN_POINT ( 'NONE',  ( 1.655952806101427033, -3.662737355149048302, -1.182683869819604841E-14 ) ) ;
#287 = CARTESIAN_POINT ( 'NONE',  ( 50.02271294988511841, 54.49948385550240459, 6.000000000000000888 ) ) ;
#288 = CARTESIAN_POINT ( 'NONE',  ( 44.03140696652198471, 47.80051614449764941, 4.306917132069485454 ) ) ;
#289 = CARTESIAN_POINT ( 'NONE',  ( 52.25172492374527877, 63.40051614449765793, 7.007379884777203749 ) ) ;
#290 = DIRECTION ( 'NONE',  ( 1.000000000000000000, 0.000000000000000000, 0.000000000000000000 ) ) ;
#291 = DIRECTION ( 'NONE',  ( 0.000000000000000000, -1.000000000000000000, 0.000000000000000000 ) ) ;
#292 = CARTESIAN_POINT ( 'NONE',  ( 47.70284917648459100, 59.60051614449765367, 6.992620115222796251 ) ) ;
#293 = ORIENTED_EDGE ( 'NONE', *, *, #1456, .F. ) ;
#294 = CARTESIAN_POINT ( 'NONE',  ( 20.00000000000000000, -20.00000000000000000, -23.00000000000000000 ) ) ;
#295 = ORIENTED_EDGE ( 'NONE', *, *, #8457, .F. ) ;
#296 = CARTESIAN_POINT ( 'NONE',  ( 0.000000000000000000, 0.000000000000000000, 0.000000000000000000 ) ) ;
#297 = ADVANCED_FACE ( 'NONE', ( #10786 ), #7829, .T. ) ;
#298 = DIRECTION ( 'NONE',  ( 1.000000000000000000, 0.000000000000000000, 0.000000000000000000 ) ) ;
#299 = DIRECTION ( 'NONE',  ( -0.000000000000000000, -0.000000000000000000, -1.000000000000000000 ) ) ;
#300 = CARTESIAN_POINT ( 'NONE',  ( 55.94051828345050836, 55.79948385550238044, -4.345558710429104465 ) ) ;
#301 = CARTESIAN_POINT ( 'NONE',  ( 2.805705207896068476, -3.226868319750173075, -3.503898532754370354 ) ) ;
#302 = CARTESIAN_POINT ( 'NONE',  ( 48.07319477248762496, 60.40051614449765793, -6.007379884777208190 ) ) ;
#303 = AXIS2_PLACEMENT_3D ( 'NONE', #3624, #7847, #12122 ) ;
#304 = CARTESIAN_POINT ( 'NONE',  ( 9.999999999999994671, 20.00000000000001421, 15.00000000000000000 ) ) ;
#305 = DIRECTION ( 'NONE',  ( 0.000000000000000000, 0.000000000000000000, -1.000000000000000000 ) ) ;
#306 = FILL_AREA_STYLE ('',( #2314 ) ) ;
#307 = CARTESIAN_POINT ( 'NONE',  ( 56.65037692655918988, 63.89948385550239607, -2.184720259617163762 ) ) ;
#308 = FACE_OUTER_BOUND ( 'NONE', #7358, .T. ) ;
#309 = ORIENTED_EDGE ( 'NONE', *, *, #197, .T. ) ;
#310 = CIRCLE ( 'NONE', #5415, 1.499999999999999778 ) ;
#311 = ORIENTED_EDGE ( 'NONE', *, *, #8812, .T. ) ;
#312 = AXIS2_PLACEMENT_3D ( 'NONE', #6238, #11325, #3101 ) ;
#313 = ORIENTED_EDGE ( 'NONE', *, *, #6610, .T. ) ;
#314 = DIRECTION ( 'NONE',  ( -0.000000000000000000, -0.000000000000000000, -1.000000000000000000 ) ) ;
#315 = CIRCLE ( 'NONE', #7843, 5.371010071662833063 ) ;
#316 = DIRECTION ( 'NONE',  ( -0.000000000000000000, 1.000000000000000000, 1.224646799147353207E-16 ) ) ;
#317 = DIRECTION ( 'NONE',  ( -0.000000000000000000, -0.000000000000000000, 1.000000000000000000 ) ) ;
#318 =( NAMED_UNIT ( * ) PLANE_ANGLE_UNIT ( ) SI_UNIT ( $, .RADIAN. ) );
#319 = CARTESIAN_POINT ( 'NONE',  ( -9.999999999999994671, 20.00000000000001421, -9.999999999999998224 ) ) ;
#320 = FACE_BOUND ( 'NONE', #11284, .T. ) ;
#321 = CARTESIAN_POINT ( 'NONE',  ( 50.02271294988512551, 54.49948385550240459, 7.000000000000000888 ) ) ;
#322 = TOROIDAL_SURFACE ( 'NONE', #9170, 5.384454397937118664, 0.5155456020628804703 ) ;
#323 = CARTESIAN_POINT ( 'NONE',  ( 56.66441430157294690, 54.90051614449765793, -2.141517661632166281 ) ) ;
#324 = DIRECTION ( 'NONE',  ( 0.000000000000000000, 0.000000000000000000, 1.000000000000000000 ) ) ;
#325 = EDGE_CURVE ( 'NONE', #12408, #8324, #8870, .T. ) ;
#326 = CARTESIAN_POINT ( 'NONE',  ( 45.90387839640214196, 54.69948385550240744, 5.676469297603166098 ) ) ;
#327 = CARTESIAN_POINT ( 'NONE',  ( 55.94051828345050836, 49.79948385550240175, -4.345558710429104465 ) ) ;
#328 = CIRCLE ( 'NONE', #10491, 0.7500000000000000000 ) ;
#329 = CARTESIAN_POINT ( 'NONE',  ( 50.02271294988513972, 64.49948385550239038, 8.000000000000001776 ) ) ;
#330 = ORIENTED_EDGE ( 'NONE', *, *, #7102, .T. ) ;
#331 = VERTEX_POINT ( 'NONE', #13575 ) ;
#332 = ORIENTED_EDGE ( 'NONE', *, *, #7882, .F. ) ;
#333 = LINE ( 'NONE', #7675, #5864 ) ;
#334 = AXIS2_PLACEMENT_3D ( 'NONE', #11503, #2020, #12598 ) ;
#335 = CARTESIAN_POINT ( 'NONE',  ( -11.49038105676659249, -12.50000000000003020, -9.000000000000000000 ) ) ;
#336 = CARTESIAN_POINT ( 'NONE',  ( 48.07319477248762496, 54.40051614449765793, -6.007379884777208190 ) ) ;
#337 = CARTESIAN_POINT ( 'NONE',  ( 47.74827507625470702, 64.40051614449765793, -7.007379884777204637 ) ) ;
#338 = CARTESIAN_POINT ( 'NONE',  ( 56.79116909180255135, 49.79948385550240175, -4.963592699179005585 ) ) ;
#339 = CARTESIAN_POINT ( 'NONE',  ( 43.33558569842703179, 59.09948385550240602, -2.141517661632099223 ) ) ;
#340 = CARTESIAN_POINT ( 'NONE',  ( 2.000000000000000000, 1.773042676681340524, -2.059984127722458425E-15 ) ) ;
#341 = EDGE_CURVE ( 'NONE', #7290, #12675, #5666, .T. ) ;
#342 = CARTESIAN_POINT ( 'NONE',  ( 47.42335538002180328, 60.40051614449765793, -8.007379884777206414 ) ) ;
#343 = EDGE_CURVE ( 'NONE', #10107, #1320, #11620, .T. ) ;
#344 = ORIENTED_EDGE ( 'NONE', *, *, #1521, .T. ) ;
#345 = VERTEX_POINT ( 'NONE', #12614 ) ;
#346 = ORIENTED_EDGE ( 'NONE', *, *, #2293, .T. ) ;
#347 = VERTEX_POINT ( 'NONE', #8345 ) ;
#348 = AXIS2_PLACEMENT_3D ( 'NONE', #13063, #10988, #12044 ) ;
#349 = DIRECTION ( 'NONE',  ( 1.000000000000000000, 0.000000000000000000, 0.000000000000000000 ) ) ;
#350 = PRESENTATION_STYLE_ASSIGNMENT (( #7830 ) ) ;
#351 = CARTESIAN_POINT ( 'NONE',  ( -74.99999999999997158, 45.00000000000001421, 15.00000000000000000 ) ) ;
#352 = CARTESIAN_POINT ( 'NONE',  ( -12.50000000000000000, 15.00000000000001599, 9.000000000000000000 ) ) ;
#353 = CARTESIAN_POINT ( 'NONE',  ( 53.50833635130540955, 59.69948385550240744, -4.867452303228209765 ) ) ;
#354 = CARTESIAN_POINT ( 'NONE',  ( 43.34962307344078880, 50.10051614449766078, -2.184720259617096705 ) ) ;
#355 = CARTESIAN_POINT ( 'NONE',  ( 52.57664461997821093, 55.40051614449767214, 8.007379884777206414 ) ) ;
#356 = CARTESIAN_POINT ( 'NONE',  ( 0.3126073911696407026, -2.020725942163686728, 3.500000000000000444 ) ) ;
#357 = DIRECTION ( 'NONE',  ( 0.000000000000000000, -0.000000000000000000, 1.000000000000000000 ) ) ;
#358 = CIRCLE ( 'NONE', #5021, 12.49999999999999645 ) ;
#359 = CARTESIAN_POINT ( 'NONE',  ( 52.29715082351538769, 62.60051614449766078, -6.992620115222796251 ) ) ;
#360 = EDGE_CURVE ( 'NONE', #407, #11356, #13500, .T. ) ;
#361 = ORIENTED_EDGE ( 'NONE', *, *, #4832, .F. ) ;
#362 = DIRECTION ( 'NONE',  ( 0.000000000000000000, 0.000000000000000000, 1.000000000000000000 ) ) ;
#363 = ORIENTED_EDGE ( 'NONE', *, *, #770, .T. ) ;
#364 = DIRECTION ( 'NONE',  ( 0.000000000000000000, 0.000000000000000000, -1.000000000000000000 ) ) ;
#365 = CARTESIAN_POINT ( 'NONE',  ( 2.000000000000000000, 0.000000000000000000, 0.000000000000000000 ) ) ;
#366 = CARTESIAN_POINT ( 'NONE',  ( -75.00000000000001421, -2.602085213965211904E-14, 0.000000000000000000 ) ) ;
#367 = CARTESIAN_POINT ( 'NONE',  ( -20.00000000000000000, -19.99999999999999289, -27.00000000000000355 ) ) ;
#368 = CARTESIAN_POINT ( 'NONE',  ( 47.74827507625478518, 54.59948385550239180, 7.007379884777227730 ) ) ;
#369 = CARTESIAN_POINT ( 'NONE',  ( 44.91013252490150620, 58.20051614449766220, -3.727524721679154940 ) ) ;
#370 = LINE ( 'NONE', #9650, #12630 ) ;
#371 = CARTESIAN_POINT ( 'NONE',  ( 6.367873360227556567, 2.886751345948123770, -5.000000000000000000 ) ) ;
#372 = CARTESIAN_POINT ( 'NONE',  ( 43.33558569842706021, 45.90051614449765793, 2.141517661632167169 ) ) ;
#373 = CARTESIAN_POINT ( 'NONE',  ( 55.71335778527780747, 46.09948385550240602, 1.832500667257165983 ) ) ;
#374 = CARTESIAN_POINT ( 'NONE',  ( 4.000000000000003553, -2.309401076758513138, -3.504271511726786859 ) ) ;
#375 = ORIENTED_EDGE ( 'NONE', *, *, #2646, .F. ) ;
#376 = ORIENTED_EDGE ( 'NONE', *, *, #3505, .F. ) ;
#377 = ORIENTED_EDGE ( 'NONE', *, *, #754, .F. ) ;
#378 = DIRECTION ( 'NONE',  ( 0.000000000000000000, 0.000000000000000000, -1.000000000000000000 ) ) ;
#379 = LINE ( 'NONE', #9030, #7198 ) ;
#380 = CARTESIAN_POINT ( 'NONE',  ( -9.999999999999994671, 20.00000000000001421, -15.00000000000000000 ) ) ;
#381 = CARTESIAN_POINT ( 'NONE',  ( -3.734041964264191549, -23.01611183630746638, -9.999999999999994671 ) ) ;
#382 = DIRECTION ( 'NONE',  ( 0.000000000000000000, 0.000000000000000000, 1.000000000000000000 ) ) ;
#383 = ADVANCED_BREP_SHAPE_REPRESENTATION ( '', ( #5648, #430 ), #3304 ) ;
#384 = CARTESIAN_POINT ( 'NONE',  ( 44.05948171654945611, 52.20051614449764799, -4.345558710429044069 ) ) ;
#385 = CARTESIAN_POINT ( 'NONE',  ( 1.267864665261691752E-11, -20.00000000000000000, 9.999999999999998224 ) ) ;
#386 = CARTESIAN_POINT ( 'NONE',  ( 55.94051828345050836, 49.79948385550240175, -4.345558710429104465 ) ) ;
#387 = CARTESIAN_POINT ( 'NONE',  ( 57.36023556966787851, 47.99948385550239038, -0.02388180880522424582 ) ) ;
#388 = CARTESIAN_POINT ( 'NONE',  ( 58.41169779390614281, 59.99948385550241170, -0.02388180880523160798 ) ) ;
#389 = ORIENTED_EDGE ( 'NONE', *, *, #8812, .F. ) ;
#390 = ORIENTED_EDGE ( 'NONE', *, *, #9083, .T. ) ;
#391 = DIRECTION ( 'NONE',  ( 1.000000000000000000, 3.469446951953615175E-16, 0.000000000000000000 ) ) ;
#392 = ORIENTED_EDGE ( 'NONE', *, *, #1283, .T. ) ;
#393 = CARTESIAN_POINT ( 'NONE',  ( 0.02944718078426972890, -0.6813962075686093023, 3.500000000000000000 ) ) ;
#394 = AXIS2_PLACEMENT_3D ( 'NONE', #8294, #11541, #12425 ) ;
#395 = ADVANCED_FACE ( 'NONE', ( #9439 ), #5005, .T. ) ;
#396 = CARTESIAN_POINT ( 'NONE',  ( 0.000000000000000000, 0.000000000000000000, -1.000000000000000000 ) ) ;
#397=STYLED_ITEM('',(#13705),#5648);
#398 = CARTESIAN_POINT ( 'NONE',  ( 48.02776887271750184, 55.60051614449765367, 5.992620115222795363 ) ) ;
#399 = CARTESIAN_POINT ( 'NONE',  ( 45.86712807150329496, 63.70051614449766220, 5.649768623646139964 ) ) ;
#400 = CARTESIAN_POINT ( 'NONE',  ( 49.97728705011486738, 51.49948385550240459, -8.000000000000001776 ) ) ;
#401 = CARTESIAN_POINT ( 'NONE',  ( 54.13287192849676188, 56.29948385550240175, 5.649768623646098220 ) ) ;
#402 = CARTESIAN_POINT ( 'NONE',  ( 13.67449106481161003, -13.83491329190030861, 9.000000000000000000 ) ) ;
#403 = CARTESIAN_POINT ( 'NONE',  ( 56.81924384183006538, 60.80051614449766362, -4.924951120819380357 ) ) ;
#404 = AXIS2_PLACEMENT_3D ( 'NONE', #167, #4383, #2039 ) ;
#405 = ORIENTED_EDGE ( 'NONE', *, *, #12351, .T. ) ;
#406 = EDGE_LOOP ( 'NONE', ( #1718, #12566, #1882, #5438, #12135, #10903, #5270, #9079, #3095, #9271, #9064, #5318 ) ) ;
#407 = VERTEX_POINT ( 'NONE', #11378 ) ;
#408 = VERTEX_POINT ( 'NONE', #12548 ) ;
#409 = DIRECTION ( 'NONE',  ( -0.000000000000000000, -0.000000000000000000, 1.000000000000000000 ) ) ;
#410 = CARTESIAN_POINT ( 'NONE',  ( -3.098410542199071749, -7.060458129626440815, -1.000000000000000000 ) ) ;
#411 = DIRECTION ( 'NONE',  ( -0.000000000000000000, -0.000000000000000000, -1.000000000000000000 ) ) ;
#412 = CARTESIAN_POINT ( 'NONE',  ( 49.97728705011488870, 53.49948385550240459, -6.000000000000000888 ) ) ;
#413 = CARTESIAN_POINT ( 'NONE',  ( 56.13503143586221000, 44.82443585060838132, -3.788959942617806220 ) ) ;
#414 = CARTESIAN_POINT ( 'NONE',  ( 56.79116909180259398, 53.20051614449766220, 4.963592699178938972 ) ) ;
#415 = CARTESIAN_POINT ( 'NONE',  ( -6.165086708099452473, -33.67449106481171128, 9.000000000000000000 ) ) ;
#416 = CARTESIAN_POINT ( 'NONE',  ( 14.92500000000001492, -21.49812382665770727, -9.000000000000000000 ) ) ;
#417 = EDGE_CURVE ( 'NONE', #8657, #10456, #8533, .T. ) ;
#418 = CARTESIAN_POINT ( 'NONE',  ( 54.13287192849671214, 60.70051614449766220, -5.649768623646139964 ) ) ;
#419 = ORIENTED_EDGE ( 'NONE', *, *, #10834, .F. ) ;
#420 = CARTESIAN_POINT ( 'NONE',  ( 1.287237434362044075, 3.875615274277557809, -3.430618716626812059 ) ) ;
#421 = AXIS2_PLACEMENT_3D ( 'NONE', #8685, #3491, #5379 ) ;
#422 = CARTESIAN_POINT ( 'NONE',  ( -2.805705207896067144, 3.226868319750155312, -3.503898532754364581 ) ) ;
#423 = ORIENTED_EDGE ( 'NONE', *, *, #11853, .T. ) ;
#424 = DIRECTION ( 'NONE',  ( 0.6040472319084893016, -0.7969485188038759604, -1.107688701425240097E-17 ) ) ;
#425 = CARTESIAN_POINT ( 'NONE',  ( 4.055492966679490330, -2.385006769472456156, -3.005124364834284023 ) ) ;
#426 = EDGE_CURVE ( 'NONE', #3623, #2660, #6766, .T. ) ;
#427 = EDGE_CURVE ( 'NONE', #5687, #966, #2944, .T. ) ;
#428 = CARTESIAN_POINT ( 'NONE',  ( 0.000000000000000000, 0.000000000000000000, 0.000000000000000000 ) ) ;
#429 = CARTESIAN_POINT ( 'NONE',  ( 52.29715082351547295, 60.39948385550239607, 6.992620115222774047 ) ) ;
#430 = AXIS2_PLACEMENT_3D ( 'NONE', #5828, #10990, #3471 ) ;
#431 = AXIS2_PLACEMENT_3D ( 'NONE', #2374, #4459, #11719 ) ;
#432 = B_SPLINE_CURVE_WITH_KNOTS ( 'NONE', 3,
 ( #8361, #5121, #6237, #1776, #4000, #1847, #9330, #10495, #8225, #2893, #12497, #7046, #11256, #8155, #2966, #799 ),
 .UNSPECIFIED., .F., .F.,
 ( 4, 3, 3, 3, 3, 4 ),
 ( 0.000000000000000000, 3.315506744709148100E-05, 6.608280158698798419E-05, 0.0001026520855291344940, 0.0001376952025664800986, 0.0001398064759190609653 ),
 .UNSPECIFIED. ) ;
#433 = CARTESIAN_POINT ( 'NONE',  ( 43.69122665457040000, 56.00051614449765935, -0.02388180880515696977 ) ) ;
#434 = CARTESIAN_POINT ( 'NONE',  ( 4.050536630291693641, -3.778525289263164222, -0.5912575323401421112 ) ) ;
#435 = DIRECTION ( 'NONE',  ( 0.9829867750086872524, 0.1836763462126260182, -1.475957441759982183E-22 ) ) ;
#436 = CARTESIAN_POINT ( 'NONE',  ( 55.71335778527780036, 62.90051614449765083, -1.832500667257213056 ) ) ;
#437 = CARTESIAN_POINT ( 'NONE',  ( 55.08986747509847248, 45.79948385550240886, -3.727524721679197572 ) ) ;
#438 = DIRECTION ( 'NONE',  ( -1.000000000000000000, 1.734723475976806848E-16, 0.000000000000000000 ) ) ;
#439 = VERTEX_POINT ( 'NONE', #5171 ) ;
#440 = APPLICATION_CONTEXT ( 'automotive_design' ) ;
#441 = ORIENTED_EDGE ( 'NONE', *, *, #10942, .F. ) ;
#442 = CARTESIAN_POINT ( 'NONE',  ( 2.449293598294706513E-15, -20.00000000000000000, 9.000000000000000000 ) ) ;
#443 = PRODUCT ( 'socket head cap screw_iso_ISO 4762 M4 x 10 - 10N', 'socket head cap screw_iso_ISO 4762 M4 x 10 - 10N', '', ( #4109 ) ) ;
#444 = CARTESIAN_POINT ( 'NONE',  ( 1.243802165048773611, -3.900692638707475624, -3.223146290109810241 ) ) ;
#445 = DIRECTION ( 'NONE',  ( 0.000000000000000000, 0.000000000000000000, -1.000000000000000000 ) ) ;
#446 = ADVANCED_FACE ( 'NONE', ( #3219 ), #7312, .F. ) ;
#447 = CARTESIAN_POINT ( 'NONE',  ( -62.49999999999997158, 32.50000000000001421, 15.00000000000000000 ) ) ;
#448 = FACE_OUTER_BOUND ( 'NONE', #5406, .T. ) ;
#449 = CARTESIAN_POINT ( 'NONE',  ( 52.29715082351538769, 54.60051614449766788, -6.992620115222796251 ) ) ;
#450 = CARTESIAN_POINT ( 'NONE',  ( 0.000000000000000000, 0.000000000000000000, -10.00000000000000000 ) ) ;
#451 = CARTESIAN_POINT ( 'NONE',  ( 55.96859303347804371, 54.19948385550240033, 4.306917132069425946 ) ) ;
#452 = CARTESIAN_POINT ( 'NONE',  ( 55.96859303347804371, 50.19948385550240744, 4.306917132069425946 ) ) ;
#453 = CIRCLE ( 'NONE', #6010, 5.000000000000000888 ) ;
#454 = ADVANCED_FACE ( 'NONE', ( #10541 ), #10406, .F. ) ;
#455 = CARTESIAN_POINT ( 'NONE',  ( 57.36023556966787851, 45.99948385550238328, -0.02388180880522424582 ) ) ;
#456 = EDGE_LOOP ( 'NONE', ( #11196, #2752, #9623, #6234 ) ) ;
#457 = ORIENTED_EDGE ( 'NONE', *, *, #5953, .F. ) ;
#458 = DIRECTION ( 'NONE',  ( -0.000000000000000000, -0.000000000000000000, -1.000000000000000000 ) ) ;
#459 = ORIENTED_EDGE ( 'NONE', *, *, #1514, .T. ) ;
#460 = CARTESIAN_POINT ( 'NONE',  ( -31.74999999999995737, 0.000000000000000000, 3.500000000000000000 ) ) ;
#461 = VECTOR ( 'NONE', #11830, 1000.000000000000000 ) ;
#462 = AXIS2_PLACEMENT_3D ( 'NONE', #7697, #5493, #290 ) ;
#463 = DIRECTION ( 'NONE',  ( -0.000000000000000000, -0.000000000000000000, 1.000000000000000000 ) ) ;
#464 = CARTESIAN_POINT ( 'NONE',  ( 50.02271294988506156, 52.50051614449766646, -6.000000000000000888 ) ) ;
#465 = CARTESIAN_POINT ( 'NONE',  ( 0.3126073911696451990, -4.041451884327386779, -1.834154111220703958E-17 ) ) ;
#466 = CARTESIAN_POINT ( 'NONE',  ( 52.62207051974839089, 50.39948385550241738, 7.992620115222770494 ) ) ;
#467 = CARTESIAN_POINT ( 'NONE',  ( 43.34962307344081012, 58.89948385550241028, 2.184720259617164650 ) ) ;
#468 = DIRECTION ( 'NONE',  ( 0.000000000000000000, 1.000000000000000000, 0.000000000000000000 ) ) ;
#469 = CARTESIAN_POINT ( 'NONE',  ( 45.31609314410960820, 64.30051614449766362, -6.485486291978072693 ) ) ;
#470 = VECTOR ( 'NONE', #11867, 1000.000000000000000 ) ;
#471 = AXIS2_PLACEMENT_3D ( 'NONE', #11512, #1111, #6405 ) ;
#472 = ORIENTED_EDGE ( 'NONE', *, *, #2154, .T. ) ;
#473 = ORIENTED_EDGE ( 'NONE', *, *, #13349, .F. ) ;
#474 = ORIENTED_EDGE ( 'NONE', *, *, #8307, .F. ) ;
#475 = ORIENTED_EDGE ( 'NONE', *, *, #7215, .F. ) ;
#476 = DIRECTION ( 'NONE',  ( -1.000000000000000000, 0.000000000000000000, 0.000000000000000000 ) ) ;
#477 = DIRECTION ( 'NONE',  ( 0.000000000000000000, 0.000000000000000000, 1.000000000000000000 ) ) ;
#478 = CARTESIAN_POINT ( 'NONE',  ( -0.9999999999999976685, -20.00000000000000000, 8.999999999999998224 ) ) ;
#479 = CARTESIAN_POINT ( 'NONE',  ( 48.07319477248768180, 54.59948385550240602, 6.007379884777225953 ) ) ;
#480 = CARTESIAN_POINT ( 'NONE',  ( 42.63976443033212149, 48.00051614449766646, -0.02388180880514948964 ) ) ;
#481 = CARTESIAN_POINT ( 'NONE',  ( 52.62207051974829852, 54.60051614449766788, -7.992620115222797139 ) ) ;
#482 = VECTOR ( 'NONE', #7003, 1000.000000000000000 ) ;
#483 = DIRECTION ( 'NONE',  ( -1.000000000000000000, 0.000000000000000000, 0.000000000000000000 ) ) ;
#484 = DIRECTION ( 'NONE',  ( -1.000000000000000000, -0.000000000000000000, -0.000000000000000000 ) ) ;
#485 = CARTESIAN_POINT ( 'NONE',  ( 45.90387839640208512, 64.30051614449766362, -5.676469297603124353 ) ) ;
#486 = VERTEX_POINT ( 'NONE', #3975 ) ;
#487 = CARTESIAN_POINT ( 'NONE',  ( 1.000000000000000000, -14.00000000000000000, 8.999999999999998224 ) ) ;
#488 = EDGE_CURVE ( 'NONE', #4812, #10387, #3886, .T. ) ;
#489 = ORIENTED_EDGE ( 'NONE', *, *, #12347, .F. ) ;
#490 = VECTOR ( 'NONE', #3038, 1000.000000000000000 ) ;
#491 = CARTESIAN_POINT ( 'NONE',  ( 2.000000000000000000, -1.773042676681341856, 2.276824562219559311E-15 ) ) ;
#492 = FACE_OUTER_BOUND ( 'NONE', #11376, .T. ) ;
#493 = CARTESIAN_POINT ( 'NONE',  ( 2.104978517884645826E-15, -20.00000000000000000, 9.000000000000000000 ) ) ;
#494 = CARTESIAN_POINT ( 'NONE',  ( 43.33558569842703179, 55.09948385550241312, -2.141517661632099223 ) ) ;
#495 = CIRCLE ( 'NONE', #6054, 15.00000000000000000 ) ;
#496 = CARTESIAN_POINT ( 'NONE',  ( 49.97728705011494554, 57.50051614449766646, 6.000000000000000888 ) ) ;
#497 = EDGE_CURVE ( 'NONE', #9340, #10627, #13638, .T. ) ;
#498 = DIRECTION ( 'NONE',  ( 1.000000000000000000, 0.000000000000000000, 0.000000000000000000 ) ) ;
#499 = DIRECTION ( 'NONE',  ( -0.000000000000000000, 0.000000000000000000, -1.000000000000000000 ) ) ;
#500 = CARTESIAN_POINT ( 'NONE',  ( 48.02776887271750184, 63.60051614449764656, 5.992620115222795363 ) ) ;
#501 = CARTESIAN_POINT ( 'NONE',  ( 47.70284917648453415, 63.39948385550240317, -6.992620115222774047 ) ) ;
#502 = DIRECTION ( 'NONE',  ( -0.000000000000000000, -0.000000000000000000, 1.000000000000000000 ) ) ;
#503 = EDGE_CURVE ( 'NONE', #347, #12172, #6338, .T. ) ;
#504 = VERTEX_POINT ( 'NONE', #30 ) ;
#505 = EDGE_CURVE ( 'NONE', #7167, #13447, #11471, .T. ) ;
#506 = UNCERTAINTY_MEASURE_WITH_UNIT (LENGTH_MEASURE( 1.000000000000000082E-05 ), #4482, 'distance_accuracy_value', 'NONE');
#507 = ORIENTED_EDGE ( 'NONE', *, *, #8494, .T. ) ;
#508 = DIRECTION ( 'NONE',  ( -1.000000000000000000, 0.000000000000000000, 0.000000000000000000 ) ) ;
#509 = CARTESIAN_POINT ( 'NONE',  ( 3.680118525130245732, -2.494084732383344605, -0.3507732604232533524 ) ) ;
#510 = PLANE ( 'NONE',  #8859 ) ;
#511 = DIRECTION ( 'NONE',  ( -1.000000000000000000, -0.000000000000000000, 0.000000000000000000 ) ) ;
#512 = DIRECTION ( 'NONE',  ( -0.000000000000000000, -0.000000000000000000, 1.000000000000000000 ) ) ;
#513 = AXIS2_PLACEMENT_3D ( 'NONE', #5640, #5842, #553 ) ;
#514 = CARTESIAN_POINT ( 'NONE',  ( 57.36023556966787851, 57.00051614449766646, 0.02388180880515038476 ) ) ;
#515 = CARTESIAN_POINT ( 'NONE',  ( 30.00000000000000355, -40.00000000000000000, 10.00000000000000000 ) ) ;
#516 = CARTESIAN_POINT ( 'NONE',  ( 62.49999999999998579, 32.50000000000001421, 9.999999999999998224 ) ) ;
#517 = VECTOR ( 'NONE', #2587, 1000.000000000000000 ) ;
#518 = CARTESIAN_POINT ( 'NONE',  ( 43.34962307344081012, 48.89948385550240317, 2.184720259617164650 ) ) ;
#519 = CARTESIAN_POINT ( 'NONE',  ( 56.81924384183011512, 60.19948385550240744, 4.924951120819313743 ) ) ;
#520 = ORIENTED_EDGE ( 'NONE', *, *, #4096, .T. ) ;
#521 = EDGE_LOOP ( 'NONE', ( #1458, #5060, #12101, #1592, #7858 ) ) ;
#522 = DIRECTION ( 'NONE',  ( 1.000000000000000000, 0.000000000000000000, 0.000000000000000000 ) ) ;
#523 = ORIENTED_EDGE ( 'NONE', *, *, #8703, .T. ) ;
#524 = CARTESIAN_POINT ( 'NONE',  ( 1.219878473194463187, -24.84890673354692936, 9.000000000000000000 ) ) ;
#525 = CIRCLE ( 'NONE', #9155, 2.649999999999985700 ) ;
#526 = DIRECTION ( 'NONE',  ( -0.000000000000000000, -0.000000000000000000, -1.000000000000000000 ) ) ;
#527 = CARTESIAN_POINT ( 'NONE',  ( 43.69122665457040000, 64.00051614449765225, -0.02388180880515696977 ) ) ;
#528 = CARTESIAN_POINT ( 'NONE',  ( -4.204015924366189871, 1.626724848190922446, -3.610627190413390419 ) ) ;
#529 = CIRCLE ( 'NONE', #3856, 2.649999999999988809 ) ;
#530 = CARTESIAN_POINT ( 'NONE',  ( 45.27934281921075410, 53.29948385550240886, -6.458785618021043895 ) ) ;
#531 = CARTESIAN_POINT ( 'NONE',  ( 54.09612160359786515, 53.69948385550240744, -5.676469297603166098 ) ) ;
#532 = CARTESIAN_POINT ( 'NONE',  ( 5.991014884144048480, -4.770489558936219510E-15, -5.000000000000000000 ) ) ;
#533 = EDGE_CURVE ( 'NONE', #8787, #7994, #6142, .T. ) ;
#534 = CARTESIAN_POINT ( 'NONE',  ( 42.39856655714564226, 62.10051614449765367, -2.493737253992044156 ) ) ;
#535 = ORIENTED_EDGE ( 'NONE', *, *, #11080, .F. ) ;
#536 = CONTEXT_DEPENDENT_SHAPE_REPRESENTATION ( #4258, #10519 ) ;
#537 = ORIENTED_EDGE ( 'NONE', *, *, #7115, .F. ) ;
#538 = ORIENTED_EDGE ( 'NONE', *, *, #13172, .T. ) ;
#539 = ORIENTED_EDGE ( 'NONE', *, *, #10740, .F. ) ;
#540 = LINE ( 'NONE', #8995, #9886 ) ;
#541 = CARTESIAN_POINT ( 'NONE',  ( 4.180345304246196214, 2.049116244671343345, -3.591763845239305919 ) ) ;
#542 = CARTESIAN_POINT ( 'NONE',  ( 20.00000000000000000, -20.00000000000000000, -23.00000000000000000 ) ) ;
#543 = LINE ( 'NONE', #8998, #5245 ) ;
#544 = CARTESIAN_POINT ( 'NONE',  ( 51.97223112728254790, 56.39948385550241028, 5.992620115222778487 ) ) ;
#545 = CARTESIAN_POINT ( 'NONE',  ( 56.65037692655921120, 53.10051614449766078, 2.184720259617097593 ) ) ;
#546 = CARTESIAN_POINT ( 'NONE',  ( 41.58830220609386430, 54.00051614449765935, -0.02388180880514929535 ) ) ;
#547 = DIRECTION ( 'NONE',  ( -1.000000000000000000, -0.000000000000000000, -0.000000000000000000 ) ) ;
#548 = CARTESIAN_POINT ( 'NONE',  ( 75.00000000000000000, 32.50000000000001421, 15.00000000000000000 ) ) ;
#549 = CARTESIAN_POINT ( 'NONE',  ( 43.33558569842706021, 63.90051614449765793, 2.141517661632167169 ) ) ;
#550 = EDGE_LOOP ( 'NONE', ( #6090, #11710, #2732, #9938 ) ) ;
#551 = FACE_OUTER_BOUND ( 'NONE', #4902, .T. ) ;
#552 = EDGE_LOOP ( 'NONE', ( #11570, #2557, #1287, #708 ) ) ;
#553 = DIRECTION ( 'NONE',  ( 1.000000000000000000, 0.000000000000000000, 0.000000000000000000 ) ) ;
#554 = CARTESIAN_POINT ( 'NONE',  ( 2.449293598294706513E-15, -20.00000000000000000, 9.000000000000000000 ) ) ;
#555 = CIRCLE ( 'NONE', #9633, 5.000000000000000888 ) ;
#556 = CARTESIAN_POINT ( 'NONE',  ( 55.96859303347804371, 58.19948385550241454, 4.306917132069425946 ) ) ;
#557 = CARTESIAN_POINT ( 'NONE',  ( 43.33558569842703179, 55.09948385550241312, -2.141517661632099223 ) ) ;
#558 = VECTOR ( 'NONE', #2702, 1000.000000000000000 ) ;
#559 = DIRECTION ( 'NONE',  ( -0.000000000000000000, -0.000000000000000000, 1.000000000000000000 ) ) ;
#560 = ADVANCED_FACE ( 'NONE', ( #5371 ), #7377, .F. ) ;
#561 = CARTESIAN_POINT ( 'NONE',  ( -1.498123826657861590, -5.075000000000000178, 9.000000000000000000 ) ) ;
#562 = PLANE ( 'NONE',  #11679 ) ;
#563 = CARTESIAN_POINT ( 'NONE',  ( 44.03140696652198471, 45.80051614449764230, 4.306917132069485454 ) ) ;
#564 = CARTESIAN_POINT ( 'NONE',  ( 47.70284917648453415, 65.39948385550239607, -6.992620115222774047 ) ) ;
#565 = DIRECTION ( 'NONE',  ( -1.000000000000000000, 0.000000000000000000, 0.000000000000000000 ) ) ;
#566 = EDGE_LOOP ( 'NONE', ( #6329, #10316, #10441 ) ) ;
#567 = ORIENTED_EDGE ( 'NONE', *, *, #10818, .T. ) ;
#568 = VERTEX_POINT ( 'NONE', #5098 ) ;
#569 = DIRECTION ( 'NONE',  ( 1.000000000000000000, 0.000000000000000000, 0.000000000000000000 ) ) ;
#570 = DIRECTION ( 'NONE',  ( -1.000000000000000000, 0.000000000000000000, 0.000000000000000000 ) ) ;
#571 = CARTESIAN_POINT ( 'NONE',  ( -5.560781378645573980, 0.000000000000000000, -4.000000000000000000 ) ) ;
#572 = CARTESIAN_POINT ( 'NONE',  ( 2.000000000000000000, -1.773042676681341856, 2.276824562219559311E-15 ) ) ;
#573 = DIRECTION ( 'NONE',  ( -0.000000000000000000, -0.000000000000000000, -1.000000000000000000 ) ) ;
#574 = CARTESIAN_POINT ( 'NONE',  ( 54.09612160359792199, 61.30051614449766362, 5.676469297603124353 ) ) ;
#575 = LINE ( 'NONE', #4688, #3098 ) ;
#576 = LINE ( 'NONE', #13235, #12689 ) ;
#577 = CARTESIAN_POINT ( 'NONE',  ( 45.90387839640214196, 60.69948385550240033, 5.676469297603166098 ) ) ;
#578 = CARTESIAN_POINT ( 'NONE',  ( 47.74827507625478518, 50.59948385550238470, 7.007379884777227730 ) ) ;
#579 = VERTEX_POINT ( 'NONE', #9306 ) ;
#580 = ORIENTED_EDGE ( 'NONE', *, *, #12965, .T. ) ;
#581 = CARTESIAN_POINT ( 'NONE',  ( 50.00000000000000000, 40.00000000000000000, 4.000000000000003553 ) ) ;
#582 = VERTEX_POINT ( 'NONE', #4050 ) ;
#583 = CARTESIAN_POINT ( 'NONE',  ( -30.00000000000000000, -39.99999999999998579, -10.00000000000000000 ) ) ;
#584 = CARTESIAN_POINT ( 'NONE',  ( 4.000000000000000000, 2.309401076758497151, -5.000000000000000000 ) ) ;
#585 = EDGE_CURVE ( 'NONE', #579, #13009, #3012, .T. ) ;
#586 = CARTESIAN_POINT ( 'NONE',  ( 51.92680522751238925, 59.40051614449765793, 6.007379884777208190 ) ) ;
#587 = EDGE_CURVE ( 'NONE', #10229, #12054, #9700, .T. ) ;
#588 = CYLINDRICAL_SURFACE ( 'NONE', #12577, 2.500000000000000444 ) ;
#589 = CARTESIAN_POINT ( 'NONE',  ( 50.02271294988513972, 62.49948385550240459, 8.000000000000001776 ) ) ;
#590 = EDGE_CURVE ( 'NONE', #178, #4538, #10739, .T. ) ;
#591 = CARTESIAN_POINT ( 'NONE',  ( 43.34962307344081012, 62.89948385550241028, 2.184720259617164650 ) ) ;
#592 = CARTESIAN_POINT ( 'NONE',  ( -4.024497503033519941, 2.323544716729375459, -3.572167766733379768 ) ) ;
#593 = CARTESIAN_POINT ( 'NONE',  ( 43.20883090819745576, 50.79948385550240175, 4.963592699179006473 ) ) ;
#594 = VERTEX_POINT ( 'NONE', #8606 ) ;
#595 = ORIENTED_EDGE ( 'NONE', *, *, #9564, .F. ) ;
#596 = ORIENTED_EDGE ( 'NONE', *, *, #7970, .T. ) ;
#597 = CIRCLE ( 'NONE', #11881, 12.50000000000000000 ) ;
#598 = ORIENTED_EDGE ( 'NONE', *, *, #2180, .F. ) ;
#599 = CARTESIAN_POINT ( 'NONE',  ( 0.000000000000000000, 4.330127018922190985, 2.500000000000005329 ) ) ;
#600 = DIRECTION ( 'NONE',  ( -0.000000000000000000, -0.000000000000000000, 1.000000000000000000 ) ) ;
#601 =( NAMED_UNIT ( * ) SI_UNIT ( $, .STERADIAN. ) SOLID_ANGLE_UNIT ( ) );
#602 = DIRECTION ( 'NONE',  ( 0.000000000000000000, 0.000000000000000000, 1.000000000000000000 ) ) ;
#603 = CARTESIAN_POINT ( 'NONE',  ( 1.925929944387235853E-31, 15.00000000000001599, 15.00000000000000178 ) ) ;
#604 = DIRECTION ( 'NONE',  ( 0.000000000000000000, -0.000000000000000000, 1.000000000000000000 ) ) ;
#605 = CARTESIAN_POINT ( 'NONE',  ( 51.97223112728254790, 60.39948385550241028, 5.992620115222778487 ) ) ;
#606 = CARTESIAN_POINT ( 'NONE',  ( 56.66441430157294690, 52.90051614449765793, -2.141517661632166281 ) ) ;
#607 = CARTESIAN_POINT ( 'NONE',  ( 42.38452918213190657, 61.90051614449766504, 2.450534656007115508 ) ) ;
#608 = CONICAL_SURFACE ( 'NONE', #7932, 2.055000000000000160, 0.7853981633974400633 ) ;
#609 = SURFACE_SIDE_STYLE ('',( #9146 ) ) ;
#610 = CARTESIAN_POINT ( 'NONE',  ( 2.482347295856823136E-15, -20.00000000000000000, -8.999999999999996447 ) ) ;
#611 = CARTESIAN_POINT ( 'NONE',  ( 54.09612160359792199, 63.30051614449766362, 5.676469297603124353 ) ) ;
#612 = AXIS2_PLACEMENT_3D ( 'NONE', #3177, #12770, #2130 ) ;
#614 = VERTEX_POINT ( 'NONE', #11711 ) ;
#613 = ORIENTED_EDGE ( 'NONE', *, *, #4413, .T. ) ;
#615 = DIRECTION ( 'NONE',  ( 1.000000000000000000, 0.000000000000000000, 0.000000000000000000 ) ) ;
#616 = ORIENTED_EDGE ( 'NONE', *, *, #729, .F. ) ;
#617 = AXIS2_PLACEMENT_3D ( 'NONE', #5271, #4088, #8312 ) ;
#618 = CARTESIAN_POINT ( 'NONE',  ( 0.4465819873852039379, 5.773502691896261751, 3.331019006688249527E-17 ) ) ;
#619 = DIRECTION ( 'NONE',  ( -0.000000000000000000, -0.000000000000000000, 1.000000000000000000 ) ) ;
#620 = APPLICATION_PROTOCOL_DEFINITION ( 'draft international standard', 'automotive_design', 1998, #3806 ) ;
#621 = CARTESIAN_POINT ( 'NONE',  ( 53.50833635130540955, 45.69948385550240033, -4.867452303228209765 ) ) ;
#622 = CARTESIAN_POINT ( 'NONE',  ( 56.66441430157296821, 56.09948385550240602, 2.141517661632100111 ) ) ;
#623 = EDGE_CURVE ( 'NONE', #12722, #6800, #4521, .T. ) ;
#624 = CARTESIAN_POINT ( 'NONE',  ( -62.49999999999997158, 20.00000000000001421, -15.00000000000000000 ) ) ;
#625 = DIRECTION ( 'NONE',  ( 1.000000000000000000, 0.000000000000000000, 0.000000000000000000 ) ) ;
#626 = AXIS2_PLACEMENT_3D ( 'NONE', #493, #13082, #10110 ) ;
#627 = CARTESIAN_POINT ( 'NONE',  ( -4.000000000000000000, 2.309401076758498483, -5.000000000000000000 ) ) ;
#628 = CARTESIAN_POINT ( 'NONE',  ( 53.50833635130544508, 63.30051614449767072, 4.867452303228181343 ) ) ;
#629 = CARTESIAN_POINT ( 'NONE',  ( 48.02776887271745210, 51.39948385550241028, -5.992620115222778487 ) ) ;
#630 = CIRCLE ( 'NONE', #7973, 0.7500000000000000000 ) ;
#631 = CARTESIAN_POINT ( 'NONE',  ( 13.67449106481173615, -26.16508670809940895, 0.000000000000000000 ) ) ;
#632 = ORIENTED_EDGE ( 'NONE', *, *, #4500, .T. ) ;
#633 = ORIENTED_EDGE ( 'NONE', *, *, #6574, .T. ) ;
#634 = EDGE_LOOP ( 'NONE', ( #3180, #8410, #6248, #1528, #779 ) ) ;
#635 = CYLINDRICAL_SURFACE ( 'NONE', #9025, 4.799999999999999822 ) ;
#636 = DIRECTION ( 'NONE',  ( 0.000000000000000000, 0.000000000000000000, -1.000000000000000000 ) ) ;
#637 = CARTESIAN_POINT ( 'NONE',  ( 6.327632967271008546, -3.313549392874691524, -4.260764098152702850 ) ) ;
#638 = AXIS2_PLACEMENT_3D ( 'NONE', #4966, #12214, #3848 ) ;
#639 = LINE ( 'NONE', #572, #12415 ) ;
#640 = DIRECTION ( 'NONE',  ( 1.000000000000000000, 0.000000000000000000, 0.000000000000000000 ) ) ;
#641 = CARTESIAN_POINT ( 'NONE',  ( 45.86712807150329496, 59.70051614449766220, 5.649768623646139964 ) ) ;
#642 = FACE_OUTER_BOUND ( 'NONE', #2942, .T. ) ;
#643 = CARTESIAN_POINT ( 'NONE',  ( 44.88205777487398507, 65.19948385550240744, -3.688883143319540814 ) ) ;
#644 = DIRECTION ( 'NONE',  ( 1.000000000000000000, 0.000000000000000000, 0.000000000000000000 ) ) ;
#645 = CARTESIAN_POINT ( 'NONE',  ( 44.03140696652192787, 61.19948385550239323, -4.306917132069425058 ) ) ;
#646 = CARTESIAN_POINT ( 'NONE',  ( 54.09612160359786515, 51.69948385550240744, -5.676469297603166098 ) ) ;
#647 = CARTESIAN_POINT ( 'NONE',  ( 56.66441430157296821, 50.09948385550240602, 2.141517661632100111 ) ) ;
#648 = STYLED_ITEM ( 'NONE', ( #11200 ), #1529 ) ;
#649 = CIRCLE ( 'NONE', #11718, 2.055000000000000160 ) ;
#650 = ORIENTED_EDGE ( 'NONE', *, *, #12597, .T. ) ;
#651 = VERTEX_POINT ( 'NONE', #1248 ) ;
#652 = CARTESIAN_POINT ( 'NONE',  ( 4.055498735588912496, -1.410041617600660491, 3.568038744583366118 ) ) ;
#653 = ORIENTED_EDGE ( 'NONE', *, *, #7184, .F. ) ;
#654 = ADVANCED_FACE ( 'NONE', ( #3348 ), #233, .F. ) ;
#655 = LINE ( 'NONE', #4833, #12685 ) ;
#656 = CARTESIAN_POINT ( 'NONE',  ( 6.481779955677435368, -2.910222513313295511, -5.040653254389411586 ) ) ;
#657 = CARTESIAN_POINT ( 'NONE',  ( 55.11794222512599362, 60.80051614449766362, -3.688883143319583446 ) ) ;
#658 = DIRECTION ( 'NONE',  ( 1.000000000000000000, 0.000000000000000000, 0.000000000000000000 ) ) ;
#659 = CARTESIAN_POINT ( 'NONE',  ( 47.37792948025162332, 61.39948385550240317, -7.992620115222770494 ) ) ;
#660 = DIRECTION ( 'NONE',  ( 1.000000000000000000, 0.000000000000000000, 0.000000000000000000 ) ) ;
#661 = DIRECTION ( 'NONE',  ( 1.000000000000000000, 0.000000000000000000, 0.000000000000000000 ) ) ;
#662 = EDGE_CURVE ( 'NONE', #1171, #9857, #2301, .T. ) ;
#663 = CARTESIAN_POINT ( 'NONE',  ( 56.79116909180255135, 47.79948385550240886, -4.963592699179005585 ) ) ;
#664 = ADVANCED_FACE ( 'NONE', ( #7703 ), #11843, .F. ) ;
#665 = ORIENTED_EDGE ( 'NONE', *, *, #7392, .F. ) ;
#666 = VECTOR ( 'NONE', #1055, 1000.000000000000000 ) ;
#667 = ORIENTED_EDGE ( 'NONE', *, *, #4356, .F. ) ;
#668 = EDGE_CURVE ( 'NONE', #3281, #8692, #12777, .T. ) ;
#669 = ORIENTED_EDGE ( 'NONE', *, *, #12070, .F. ) ;
#670 = ORIENTED_EDGE ( 'NONE', *, *, #2051, .T. ) ;
#671 = CARTESIAN_POINT ( 'NONE',  ( -0.6920835326022555245, -4.454600218803899558, -3.597382984111586079 ) ) ;
#672 = DIRECTION ( 'NONE',  ( -0.000000000000000000, 0.000000000000000000, 1.000000000000000000 ) ) ;
#673 = LINE ( 'NONE', #12175, #10645 ) ;
#674 = DIRECTION ( 'NONE',  ( 0.4999999999999977796, 0.8660254037844398178, 0.000000000000000000 ) ) ;
#675 = DIRECTION ( 'NONE',  ( -1.000000000000000000, 0.000000000000000000, 1.224646799147353207E-16 ) ) ;
#676 = CARTESIAN_POINT ( 'NONE',  ( 55.11794222512599362, 44.80051614449766362, -3.688883143319583446 ) ) ;
#677 = CARTESIAN_POINT ( 'NONE',  ( 45.86712807150329496, 53.70051614449766220, 5.649768623646139964 ) ) ;
#678 = CARTESIAN_POINT ( 'NONE',  ( 42.39856655714564226, 56.10051614449766078, -2.493737253992044156 ) ) ;
#679 = AXIS2_PLACEMENT_3D ( 'NONE', #3829, #8050, #11290 ) ;
#680 = DIRECTION ( 'NONE',  ( 0.9396926207859138680, 1.150791560227856926E-16, -0.3420201433256536139 ) ) ;
#681 = AXIS2_PLACEMENT_3D ( 'NONE', #3109, #7339, #6931 ) ;
#682 = FACE_OUTER_BOUND ( 'NONE', #4570, .T. ) ;
#683 = VECTOR ( 'NONE', #512, 1000.000000000000000 ) ;
#684 = CARTESIAN_POINT ( 'NONE',  ( 42.38452918213190657, 49.90051614449766504, 2.450534656007115508 ) ) ;
#686 = VERTEX_POINT ( 'NONE', #2504 ) ;
#685 = ORIENTED_EDGE ( 'NONE', *, *, #5886, .F. ) ;
#687 = EDGE_CURVE ( 'NONE', #7344, #3771, #10007, .T. ) ;
#688 = CARTESIAN_POINT ( 'NONE',  ( -1.747541505913277282, 3.837784562140256650, -3.503702292528906526 ) ) ;
#689 = EDGE_CURVE ( 'NONE', #12154, #1369, #11986, .T. ) ;
#690 = VERTEX_POINT ( 'NONE', #9775 ) ;
#691 = ORIENTED_EDGE ( 'NONE', *, *, #12541, .F. ) ;
#692 = CIRCLE ( 'NONE', #11545, 2.149999999999999023 ) ;
#693 = CARTESIAN_POINT ( 'NONE',  ( 0.000000000000000000, -4.330127018922193649, -2.500000000000000000 ) ) ;
#694 = CARTESIAN_POINT ( 'NONE',  ( -14.92499999999998828, -21.49812382665792754, -9.000000000000000000 ) ) ;
#695 = CIRCLE ( 'NONE', #1587, 4.000000000000000000 ) ;
#696 = APPLICATION_PROTOCOL_DEFINITION ( 'draft international standard', 'automotive_design', 1998, #9203 ) ;
#697 = CARTESIAN_POINT ( 'NONE',  ( 43.33558569842703179, 65.09948385550239891, -2.141517661632099223 ) ) ;
#698 = CARTESIAN_POINT ( 'NONE',  ( 42.63976443033212149, 58.99948385550239038, 0.02388180880522514787 ) ) ;
#699 = CARTESIAN_POINT ( 'NONE',  ( 30.00000000000000355, -40.00000000000000000, 0.000000000000000000 ) ) ;
#700 = DIRECTION ( 'NONE',  ( 0.000000000000000000, -0.000000000000000000, 1.000000000000000000 ) ) ;
#701 = DIRECTION ( 'NONE',  ( -1.000000000000000000, -0.000000000000000000, -0.000000000000000000 ) ) ;
#702 = CARTESIAN_POINT ( 'NONE',  ( 49.97728705011495265, 53.50051614449765935, 7.000000000000000888 ) ) ;
#703 = CARTESIAN_POINT ( 'NONE',  ( 51.92680522751233951, 49.59948385550241312, -6.007379884777223289 ) ) ;
#704 = CARTESIAN_POINT ( 'NONE',  ( 6.165086708099353885, -6.325508935188239867, -9.000000000000000000 ) ) ;
#705 = ORIENTED_EDGE ( 'NONE', *, *, #6210, .F. ) ;
#706 = EDGE_CURVE ( 'NONE', #10906, #10425, #3298, .T. ) ;
#707 = ADVANCED_FACE ( 'NONE', ( #3417 ), #11910, .F. ) ;
#708 = ORIENTED_EDGE ( 'NONE', *, *, #3659, .T. ) ;
#709 = EDGE_LOOP ( 'NONE', ( #11053, #4698, #8961, #667, #5980, #11825 ) ) ;
#710 = CARTESIAN_POINT ( 'NONE',  ( 0.000000000000000000, 0.000000000000000000, 0.000000000000000000 ) ) ;
#711 = DIRECTION ( 'NONE',  ( -0.7779254092217071648, -0.6283566325640553840, 0.000000000000000000 ) ) ;
#712 = CARTESIAN_POINT ( 'NONE',  ( 6.534533895392292457, -2.951347675328713116, 5.111884124469662893 ) ) ;
#713 = CARTESIAN_POINT ( 'NONE',  ( -4.999999999999998224, -20.00000000000000000, -20.00000000000000000 ) ) ;
#714 = DIRECTION ( 'NONE',  ( -0.7779254092217071648, -0.6283566325640553840, 0.000000000000000000 ) ) ;
#715 = DIRECTION ( 'NONE',  ( -1.000000000000000000, 0.000000000000000000, -0.000000000000000000 ) ) ;
#716 = CARTESIAN_POINT ( 'NONE',  ( 55.71335778527780036, 44.90051614449765793, -1.832500667257213056 ) ) ;
#717 = DIRECTION ( 'NONE',  ( 0.000000000000000000, 0.000000000000000000, -1.000000000000000000 ) ) ;
#718 = CARTESIAN_POINT ( 'NONE',  ( 43.33558569842703179, 57.09948385550240602, -2.141517661632099223 ) ) ;
#719 = CARTESIAN_POINT ( 'NONE',  ( 44.03140696652192787, 53.19948385550238612, -4.306917132069425058 ) ) ;
#720 = VERTEX_POINT ( 'NONE', #9842 ) ;
#721 = CARTESIAN_POINT ( 'NONE',  ( 44.03140696652192787, 51.19948385550238612, -4.306917132069425058 ) ) ;
#722 = ORIENTED_EDGE ( 'NONE', *, *, #11850, .F. ) ;
#723 = ORIENTED_EDGE ( 'NONE', *, *, #9205, .T. ) ;
#724 = CARTESIAN_POINT ( 'NONE',  ( 62.49999999999998579, 45.00000000000001421, -5.000000000000000000 ) ) ;
#725 = VERTEX_POINT ( 'NONE', #11778 ) ;
#726 = CIRCLE ( 'NONE', #7603, 2.649999999999985700 ) ;
#727 = CARTESIAN_POINT ( 'NONE',  ( -9.999999999999996447, 0.000000000000000000, -9.999999999999998224 ) ) ;
#728 = LINE ( 'NONE', #11257, #8503 ) ;
#729 = EDGE_CURVE ( 'NONE', #12709, #1912, #7570, .T. ) ;
#730 = DIRECTION ( 'NONE',  ( 0.000000000000000000, 0.000000000000000000, 1.000000000000000000 ) ) ;
#731 = CARTESIAN_POINT ( 'NONE',  ( 44.28664221472221385, 57.90051614449765793, 1.832500667257213722 ) ) ;
#732 = CARTESIAN_POINT ( 'NONE',  ( 4.000000000000000000, -0.8732470631449981147, -3.223155494240760088 ) ) ;
#733 = CARTESIAN_POINT ( 'NONE',  ( 42.39856655714566358, 56.89948385550240317, 2.493737253992119207 ) ) ;
#734 = CARTESIAN_POINT ( 'NONE',  ( 45.86712807150323812, 63.29948385550240886, -5.649768623646098220 ) ) ;
#735 = DIRECTION ( 'NONE',  ( -1.000000000000000000, 0.000000000000000000, 0.000000000000000000 ) ) ;
#736 = CONICAL_SURFACE ( 'NONE', #7395, 5.371010071662833063, 1.221730476396037490 ) ;
#737 = CARTESIAN_POINT ( 'NONE',  ( 54.68390685589033495, 51.69948385550241454, -6.485486291978119766 ) ) ;
#738 = ORIENTED_EDGE ( 'NONE', *, *, #10743, .T. ) ;
#739 = CIRCLE ( 'NONE', #6941, 5.000000000000000888 ) ;
#740 = EDGE_LOOP ( 'NONE', ( #13174, #5500 ) ) ;
#741 = ORIENTED_EDGE ( 'NONE', *, *, #6618, .T. ) ;
#742 = VECTOR ( 'NONE', #13525, 1000.000000000000000 ) ;
#743 = LINE ( 'NONE', #9777, #4835 ) ;
#744 = CYLINDRICAL_SURFACE ( 'NONE', #7474, 1.500000000000001332 ) ;
#745 = B_SPLINE_CURVE_WITH_KNOTS ( 'NONE', 3,
 ( #13610, #3044, #9471, #11483, #1864, #10442 ),
 .UNSPECIFIED., .F., .F.,
 ( 4, 2, 4 ),
 ( 0.000000000000000000, 0.0003657767439067419277, 0.0007315534878134838555 ),
 .UNSPECIFIED. ) ;
#746 = AXIS2_PLACEMENT_3D ( 'NONE', #10700, #7661, #9662 ) ;
#747 = CARTESIAN_POINT ( 'NONE',  ( 0.000000000000000000, 0.000000000000000000, -1.000000000000000000 ) ) ;
#748 = CARTESIAN_POINT ( 'NONE',  ( 6.534838248920899595, 5.903531555104835071, 8.098083288904839678E-18 ) ) ;
#749 = DIRECTION ( 'NONE',  ( 1.000000000000000000, 0.000000000000000000, 0.000000000000000000 ) ) ;
#750 = CARTESIAN_POINT ( 'NONE',  ( 43.69122665457040000, 64.99948385550240459, 0.02388180880521036456 ) ) ;
#751 = CARTESIAN_POINT ( 'NONE',  ( 47.74827507625470702, 52.40051614449765083, -7.007379884777204637 ) ) ;
#752 = ADVANCED_FACE ( 'NONE', ( #10939 ), #13007, .T. ) ;
#753 = CARTESIAN_POINT ( 'NONE',  ( 45.27934281921082516, 57.70051614449766930, 6.458785618021089192 ) ) ;
#754 = EDGE_CURVE ( 'NONE', #9622, #4847, #5703, .T. ) ;
#755 = CARTESIAN_POINT ( 'NONE',  ( -4.000000000000000000, 0.8576368993457507139, -3.433240632782198709 ) ) ;
#756 = CARTESIAN_POINT ( 'NONE',  ( 56.81924384183006538, 52.80051614449766362, -4.924951120819380357 ) ) ;
#758 = EDGE_LOOP ( 'NONE', ( #6496, #10523, #13430, #10250 ) ) ;
#757 = VERTEX_POINT ( 'NONE', #9640 ) ;
#759 = AXIS2_PLACEMENT_3D ( 'NONE', #12342, #851, #4126 ) ;
#760 = ORIENTED_EDGE ( 'NONE', *, *, #7579, .T. ) ;
#761 = ORIENTED_EDGE ( 'NONE', *, *, #9825, .T. ) ;
#762 = EDGE_LOOP ( 'NONE', ( #12304, #11458, #12169, #8097 ) ) ;
#763 = B_SPLINE_CURVE_WITH_KNOTS ( 'NONE', 3,
 ( #5749, #11051, #9056, #592, #12230, #1570 ),
 .UNSPECIFIED., .F., .F.,
 ( 4, 2, 4 ),
 ( -3.640115492410698714E-06, 0.0002066546034006521879, 0.0004169493222937151081 ),
 .UNSPECIFIED. ) ;
#764 = CARTESIAN_POINT ( 'NONE',  ( 4.071447262713887127, -2.020725942163686284, 3.500000000000000444 ) ) ;
#765 = DIRECTION ( 'NONE',  ( 0.000000000000000000, 0.000000000000000000, 1.000000000000000000 ) ) ;
#766 = PRODUCT_CONTEXT ( 'NONE', #12286, 'mechanical' ) ;
#767 = CARTESIAN_POINT ( 'NONE',  ( 44.91013252490152752, 46.79948385550240886, 3.727524721679198461 ) ) ;
#768 = CARTESIAN_POINT ( 'NONE',  ( 45.90387839640214196, 60.69948385550240033, 5.676469297603166098 ) ) ;
#769 = EDGE_CURVE ( 'NONE', #9673, #2278, #201, .T. ) ;
#770 = EDGE_CURVE ( 'NONE', #11811, #6957, #8397, .T. ) ;
#771 = CARTESIAN_POINT ( 'NONE',  ( 2.449293598294706513E-15, -20.00000000000000000, -20.00000000000000000 ) ) ;
#772 = CARTESIAN_POINT ( 'NONE',  ( -12.99038105676654453, -27.50000000000006040, -9.000000000000000000 ) ) ;
#773 = CARTESIAN_POINT ( 'NONE',  ( 6.534838248920897819, 2.951765777552412651, 5.112608298763836601 ) ) ;
#774 = CARTESIAN_POINT ( 'NONE',  ( 47.70284917648459100, 53.60051614449765367, 6.992620115222796251 ) ) ;
#775 = CARTESIAN_POINT ( 'NONE',  ( 44.28664221472220675, 55.09948385550241312, -1.832500667257165317 ) ) ;
#776 = DIRECTION ( 'NONE',  ( -0.000000000000000000, -0.000000000000000000, 1.000000000000000000 ) ) ;
#777 = EDGE_CURVE ( 'NONE', #10184, #6619, #3754, .T. ) ;
#778 = ORIENTED_EDGE ( 'NONE', *, *, #2180, .T. ) ;
#779 = ORIENTED_EDGE ( 'NONE', *, *, #7051, .F. ) ;
#780 = EDGE_LOOP ( 'NONE', ( #3669, #13364, #13258, #3786 ) ) ;
#781 = CARTESIAN_POINT ( 'NONE',  ( 2.449293598294706513E-15, -20.00000000000000000, -20.00000000000000000 ) ) ;
#782 = VECTOR ( 'NONE', #5023, 1000.000000000000000 ) ;
#783 = AXIS2_PLACEMENT_3D ( 'NONE', #1118, #7239, #5238 ) ;
#784 = CARTESIAN_POINT ( 'NONE',  ( 0.8816464618332836567, -24.71833652004169934, 9.999999999999998224 ) ) ;
#785 = CARTESIAN_POINT ( 'NONE',  ( 6.506987859255527695, -2.925375531177290878, 5.066899051217877314 ) ) ;
#786 = CARTESIAN_POINT ( 'NONE',  ( 49.97728705011488159, 47.49948385550240459, -7.000000000000000888 ) ) ;
#787 = DIRECTION ( 'NONE',  ( 0.000000000000000000, 0.000000000000000000, -1.000000000000000000 ) ) ;
#788 = LINE ( 'NONE', #7448, #8616 ) ;
#789 = CARTESIAN_POINT ( 'NONE',  ( 48.02776887271750184, 45.60051614449765367, 5.992620115222795363 ) ) ;
#790 = DIRECTION ( 'NONE',  ( -1.000000000000000000, 0.000000000000000000, 0.000000000000000000 ) ) ;
#791 = CARTESIAN_POINT ( 'NONE',  ( 54.09612160359786515, 55.69948385550240744, -5.676469297603166098 ) ) ;
#792 = CARTESIAN_POINT ( 'NONE',  ( 55.94051828345050836, 51.79948385550240175, -4.345558710429104465 ) ) ;
#793 = ORIENTED_EDGE ( 'NONE', *, *, #2126, .T. ) ;
#794 = CARTESIAN_POINT ( 'NONE',  ( 54.13287192849676188, 52.29948385550240886, 5.649768623646098220 ) ) ;
#795 = MECHANICAL_DESIGN_GEOMETRIC_PRESENTATION_REPRESENTATION (  '', ( #3898 ), #6353 ) ;
#796 = ORIENTED_EDGE ( 'NONE', *, *, #2151, .F. ) ;
#797 = LINE ( 'NONE', #724, #5719 ) ;
#798 = ORIENTED_EDGE ( 'NONE', *, *, #2783, .T. ) ;
#799 = CARTESIAN_POINT ( 'NONE',  ( 4.175813232069147674, 2.061359961916367833, 3.570380186727398097 ) ) ;
#800 = CARTESIAN_POINT ( 'NONE',  ( 4.688877333453708829, -18.97314589549297281, 9.999999999999998224 ) ) ;
#801 = CARTESIAN_POINT ( 'NONE',  ( 8.500000000000000000, 2.886751345948123770, -5.000000000000000000 ) ) ;
#802 = CARTESIAN_POINT ( 'NONE',  ( 43.69122665457040000, 60.00051614449765935, -0.02388180880515696977 ) ) ;
#803 = CARTESIAN_POINT ( 'NONE',  ( -13.49999999999999467, -20.00000000000005329, 9.000000000000000000 ) ) ;
#804 = CARTESIAN_POINT ( 'NONE',  ( 58.41169779390614281, 61.99948385550241170, -0.02388180880523160798 ) ) ;
#805 = CARTESIAN_POINT ( 'NONE',  ( -4.203833317240879275, -1.627343821129593859, -3.597273115243890818 ) ) ;
#806 = CARTESIAN_POINT ( 'NONE',  ( 45.31609314410967926, 50.69948385550240744, 6.485486291978119766 ) ) ;
#807 = ORIENTED_EDGE ( 'NONE', *, *, #11080, .T. ) ;
#808 = ORIENTED_EDGE ( 'NONE', *, *, #8589, .F. ) ;
#809 = ORIENTED_EDGE ( 'NONE', *, *, #4115, .T. ) ;
#810 = ADVANCED_FACE ( 'NONE', ( #3686 ), #6868, .T. ) ;
#811 = PLANE ( 'NONE',  #7708 ) ;
#812 = CARTESIAN_POINT ( 'NONE',  ( 8.759913291900563337, -32.17636723815374467, 9.000000000000000000 ) ) ;
#813 = CYLINDRICAL_SURFACE ( 'NONE', #10822, 2.149999999999999023 ) ;
#814 = CARTESIAN_POINT ( 'NONE',  ( 0.000000000000000000, 0.000000000000000000, 0.000000000000000000 ) ) ;
#815 = CARTESIAN_POINT ( 'NONE',  ( 46.49166364869460466, 64.69948385550240744, 4.867452303228209765 ) ) ;
#816 = CARTESIAN_POINT ( 'NONE',  ( 44.05948171654945611, 56.20051614449765509, -4.345558710429044069 ) ) ;
#817 = CARTESIAN_POINT ( 'NONE',  ( 52.57664461997821093, 61.40051614449765793, 8.007379884777206414 ) ) ;
#818 = CARTESIAN_POINT ( 'NONE',  ( -4.197312064133472020, -0.8182229787990021874, -3.502518405183886685 ) ) ;
#819 = CARTESIAN_POINT ( 'NONE',  ( 57.60143344285435774, 47.10051614449766078, 2.493737253992045044 ) ) ;
#820 = AXIS2_PLACEMENT_3D ( 'NONE', #10787, #8864, #7690 ) ;
#822 = VERTEX_POINT ( 'NONE', #5907 ) ;
#821 = ORIENTED_EDGE ( 'NONE', *, *, #11191, .T. ) ;
#823 = ORIENTED_EDGE ( 'NONE', *, *, #3310, .T. ) ;
#824 = ORIENTED_EDGE ( 'NONE', *, *, #3992, .T. ) ;
#825 = DIRECTION ( 'NONE',  ( -0.000000000000000000, -0.000000000000000000, 1.000000000000000000 ) ) ;
#826 = CARTESIAN_POINT ( 'NONE',  ( 0.1739375980333736638, 5.301268757141562205, -0.8179331680533008520 ) ) ;
#827 = CYLINDRICAL_SURFACE ( 'NONE', #9755, 12.49999999999999645 ) ;
#828 = APPLICATION_PROTOCOL_DEFINITION ( 'draft international standard', 'automotive_design', 1998, #440 ) ;
#829 = CARTESIAN_POINT ( 'NONE',  ( 47.74827507625478518, 64.59948385550239891, 7.007379884777227730 ) ) ;
#830 = AXIS2_PLACEMENT_3D ( 'NONE', #11462, #2962, #13381 ) ;
#831 = CARTESIAN_POINT ( 'NONE',  ( 52.29715082351547295, 56.39948385550239607, 6.992620115222774047 ) ) ;
#832 = EDGE_CURVE ( 'NONE', #7686, #1117, #3261, .T. ) ;
#833 = VECTOR ( 'NONE', #4057, 1000.000000000000000 ) ;
#834 = LINE ( 'NONE', #8057, #1573 ) ;
#835 = DIRECTION ( 'NONE',  ( 0.000000000000000000, -0.5000000000000011102, -0.8660254037844379305 ) ) ;
#836 = CARTESIAN_POINT ( 'NONE',  ( 55.48859070151218020, 45.00000000000002132, -4.999999999999993783 ) ) ;
#837 = CARTESIAN_POINT ( 'NONE',  ( 54.13287192849671214, 50.70051614449766220, -5.649768623646139964 ) ) ;
#838 = CARTESIAN_POINT ( 'NONE',  ( 49.97728705011488870, 49.49948385550241170, -6.000000000000000888 ) ) ;
#839 = CARTESIAN_POINT ( 'NONE',  ( 55.00886502606627459, 44.74918607449495767, -5.000000000000008882 ) ) ;
#840 = EDGE_CURVE ( 'NONE', #3920, #7551, #3094, .T. ) ;
#841 = EDGE_LOOP ( 'NONE', ( #7114, #472, #9760, #1503 ) ) ;
#842 = CARTESIAN_POINT ( 'NONE',  ( 14.14213562373095101, -25.00000000000000711, -50.00000000000000000 ) ) ;
#843 = AXIS2_PLACEMENT_3D ( 'NONE', #13504, #4053, #8278 ) ;
#844 = VERTEX_POINT ( 'NONE', #13077 ) ;
#846 = EDGE_CURVE ( 'NONE', #7079, #13382, #12319, .T. ) ;
#845 = ORIENTED_EDGE ( 'NONE', *, *, #3310, .F. ) ;
#847 = CARTESIAN_POINT ( 'NONE',  ( -4.000000000000000000, 2.309401076758498483, -5.000000000000000000 ) ) ;
#848 = AXIS2_PLACEMENT_3D ( 'NONE', #6811, #5853, #7015 ) ;
#849 = EDGE_CURVE ( 'NONE', #12479, #12223, #1301, .T. ) ;
#850 = AXIS2_PLACEMENT_3D ( 'NONE', #4188, #4255, #986 ) ;
#851 = DIRECTION ( 'NONE',  ( 0.000000000000000000, 0.000000000000000000, 1.000000000000000000 ) ) ;
#852 = FACE_OUTER_BOUND ( 'NONE', #11629, .T. ) ;
#853 = PRESENTATION_STYLE_ASSIGNMENT (( #8281 ) ) ;
#854 = FACE_OUTER_BOUND ( 'NONE', #10660, .T. ) ;
#855 =( GEOMETRIC_REPRESENTATION_CONTEXT ( 3 ) GLOBAL_UNCERTAINTY_ASSIGNED_CONTEXT ( ( #10887 ) ) GLOBAL_UNIT_ASSIGNED_CONTEXT ( ( #4614, #12009, #13098 ) ) REPRESENTATION_CONTEXT ( 'NONE', 'WORKASPACE' ) );
#856 = AXIS2_PLACEMENT_3D ( 'NONE', #8158, #2895, #7122 ) ;
#857 = CARTESIAN_POINT ( 'NONE',  ( -3.522875095019672109, 2.820352903225427532, -3.598441714920591394 ) ) ;
#858 = CARTESIAN_POINT ( 'NONE',  ( 51.92680522751233951, 63.59948385550239891, -6.007379884777223289 ) ) ;
#859 = CARTESIAN_POINT ( 'NONE',  ( 30.00000000000000355, 0.000000000000000000, -10.00000000000000000 ) ) ;
#860 = LINE ( 'NONE', #12748, #12328 ) ;
#861 = CARTESIAN_POINT ( 'NONE',  ( 55.96859303347804371, 56.19948385550241454, 4.306917132069425946 ) ) ;
#862 = ORIENTED_EDGE ( 'NONE', *, *, #1519, .T. ) ;
#863 = CARTESIAN_POINT ( 'NONE',  ( 44.05948171654949874, 50.79948385550238754, 4.345558710429105354 ) ) ;
#864 = EDGE_LOOP ( 'NONE', ( #11730, #7424, #1233, #7744 ) ) ;
#865 = CARTESIAN_POINT ( 'NONE',  ( -74.99999999999997158, 45.00000000000001421, -15.00000000000000000 ) ) ;
#866 = CARTESIAN_POINT ( 'NONE',  ( 3.961557105776161158, -1.423285172354515016, 3.500000000000000444 ) ) ;
#867 = AXIS2_PLACEMENT_3D ( 'NONE', #12641, #5263, #61 ) ;
#868 = ORIENTED_EDGE ( 'NONE', *, *, #8531, .T. ) ;
#869 = CARTESIAN_POINT ( 'NONE',  ( 0.9183817310753817909, -24.91493387504115020, 9.999999999999998224 ) ) ;
#870 = ADVANCED_BREP_SHAPE_REPRESENTATION ( '', ( #5623, #430 ), #7942 ) ;
#871 = FACE_OUTER_BOUND ( 'NONE', #4942, .T. ) ;
#872 = CARTESIAN_POINT ( 'NONE',  ( 55.96859303347805081, 46.19948385550240033, 4.306917132069425058 ) ) ;
#873 = CARTESIAN_POINT ( 'NONE',  ( 54.09612160359792199, 49.30051614449765651, 5.676469297603124353 ) ) ;
#874 = CARTESIAN_POINT ( 'NONE',  ( 54.23491683972284960, 45.00000000000001421, -4.999999999999999112 ) ) ;
#875 = CARTESIAN_POINT ( 'NONE',  ( 56.79116909180255135, 61.79948385550240175, -4.963592699179005585 ) ) ;
#876 = PRESENTATION_LAYER_ASSIGNMENT (  '', '', ( #9 ) ) ;
#877 = AXIS2_PLACEMENT_3D ( 'NONE', #137, #12911, #3388 ) ;
#878 = PLANE ( 'NONE',  #11324 ) ;
#879 = CARTESIAN_POINT ( 'NONE',  ( 47.42335538002188144, 48.59948385550239891, 8.007379884777233059 ) ) ;
#880 = ORIENTED_EDGE ( 'NONE', *, *, #8833, .F. ) ;
#881 = ORIENTED_EDGE ( 'NONE', *, *, #13242, .T. ) ;
#882 = ORIENTED_EDGE ( 'NONE', *, *, #6921, .F. ) ;
#883 = EDGE_CURVE ( 'NONE', #13411, #7551, #2265, .T. ) ;
#884 = DIRECTION ( 'NONE',  ( -0.000000000000000000, 0.000000000000000000, 1.000000000000000000 ) ) ;
#885 = AXIS2_PLACEMENT_3D ( 'NONE', #1429, #5608, #5539 ) ;
#886 =( LENGTH_UNIT ( ) NAMED_UNIT ( * ) SI_UNIT ( .MILLI., .METRE. ) );
#887 = CYLINDRICAL_SURFACE ( 'NONE', #10653, 1.500000000000000444 ) ;
#888 = DIRECTION ( 'NONE',  ( 0.000000000000000000, -0.000000000000000000, 1.000000000000000000 ) ) ;
#889 = DIRECTION ( 'NONE',  ( -0.7071067811865350272, 8.659560562355083235E-17, -0.7071067811865598962 ) ) ;
#890 = CARTESIAN_POINT ( 'NONE',  ( 55.71335778527780747, 60.09948385550240602, 1.832500667257165983 ) ) ;
#891 = CARTESIAN_POINT ( 'NONE',  ( 55.94051828345054389, 57.20051614449766220, 4.345558710429044957 ) ) ;
#892 = CARTESIAN_POINT ( 'NONE',  ( 42.38452918213190657, 57.90051614449765793, 2.450534656007115508 ) ) ;
#893 = DIRECTION ( 'NONE',  ( -0.000000000000000000, -0.000000000000000000, 1.000000000000000000 ) ) ;
#894 = CARTESIAN_POINT ( 'NONE',  ( 50.02271294988505446, 52.50051614449766646, -8.000000000000001776 ) ) ;
#895 = VECTOR ( 'NONE', #4344, 1000.000000000000000 ) ;
#897 = ORIENTED_EDGE ( 'NONE', *, *, #668, .F. ) ;
#896 = ORIENTED_EDGE ( 'NONE', *, *, #12447, .T. ) ;
#898 = VERTEX_POINT ( 'NONE', #4729 ) ;
#899 = EDGE_LOOP ( 'NONE', ( #12321, #1610, #650, #2100, #2554, #2982, #11409, #10105, #9169, #11499, #11268, #10678 ) ) ;
#900 = CARTESIAN_POINT ( 'NONE',  ( -6.473970235329672780E-16, -4.862606272033106691, -3.745885042887442395 ) ) ;
#901 = CARTESIAN_POINT ( 'NONE',  ( 6.420058897733097680, 2.891482565094591006, -5.008194711943424693 ) ) ;
#902 = DIRECTION ( 'NONE',  ( -1.000000000000000000, 0.000000000000000000, 0.000000000000000000 ) ) ;
#903 = DIRECTION ( 'NONE',  ( -0.04542589977017699732, 0.9989677110047501252, 0.000000000000000000 ) ) ;
#904 = AXIS2_PLACEMENT_3D ( 'NONE', #10254, #2791, #7010 ) ;
#905 = APPLICATION_PROTOCOL_DEFINITION ( 'draft international standard', 'automotive_design', 1998, #10613 ) ;
#906 = CARTESIAN_POINT ( 'NONE',  ( 49.97728705011488159, 61.49948385550240459, -7.000000000000000888 ) ) ;
#907 = AXIS2_PLACEMENT_3D ( 'NONE', #3681, #5697, #9899 ) ;
#908 = CARTESIAN_POINT ( 'NONE',  ( 43.33558569842703179, 57.09948385550240602, -2.141517661632099223 ) ) ;
#909 = VECTOR ( 'NONE', #1619, 1000.000000000000000 ) ;
#910 = EDGE_CURVE ( 'NONE', #11255, #13173, #3889, .T. ) ;
#911 = CARTESIAN_POINT ( 'NONE',  ( 54.09612160359792199, 57.30051614449765651, 5.676469297603124353 ) ) ;
#912 = CYLINDRICAL_SURFACE ( 'NONE', #2246, 12.50000000000000000 ) ;
#913 = CARTESIAN_POINT ( 'NONE',  ( -1.000000000000000000, -14.00000000000000000, 8.999999999999998224 ) ) ;
#914 = CARTESIAN_POINT ( 'NONE',  ( 0.000000000000000000, 0.000000000000000000, -4.974599999999998801 ) ) ;
#915 = CARTESIAN_POINT ( 'NONE',  ( 47.74827507625469281, 50.40051614449764372, -7.007379884777203749 ) ) ;
#916 = CARTESIAN_POINT ( 'NONE',  ( 55.71335778527780747, 50.09948385550240602, 1.832500667257165983 ) ) ;
#917 = DIRECTION ( 'NONE',  ( 1.000000000000000000, 0.000000000000000000, -0.000000000000000000 ) ) ;
#918 = ADVANCED_FACE ( 'NONE', ( #1809 ), #9970, .T. ) ;
#919 = VERTEX_POINT ( 'NONE', #5981 ) ;
#920 = CARTESIAN_POINT ( 'NONE',  ( 0.000000000000000000, 0.000000000000000000, 0.000000000000000000 ) ) ;
#921 = CIRCLE ( 'NONE', #4467, 1.500000000000000666 ) ;
#922 = ORIENTED_EDGE ( 'NONE', *, *, #10131, .F. ) ;
#923 = EDGE_LOOP ( 'NONE', ( #4335, #13115, #1965, #9708, #10853 ) ) ;
#924 = CARTESIAN_POINT ( 'NONE',  ( 2.000000000000000444, 3.464101615137754830, -3.142992957459231018 ) ) ;
#925 = CARTESIAN_POINT ( 'NONE',  ( 2.449293598294706513E-15, -20.00000000000000000, -9.000000000000000000 ) ) ;
#926 = CARTESIAN_POINT ( 'NONE',  ( 6.362374563308273778, -3.415000007734520171, -4.302769906043296011 ) ) ;
#927 = CARTESIAN_POINT ( 'NONE',  ( 2.449293598294706513E-15, -20.00000000000000000, -8.999999999999998224 ) ) ;
#928 = EDGE_CURVE ( 'NONE', #6427, #7344, #12002, .T. ) ;
#929 = DIRECTION ( 'NONE',  ( -4.082155997157844188E-16, 1.000000000000000000, 0.000000000000000000 ) ) ;
#930 = CARTESIAN_POINT ( 'NONE',  ( 44.91013252490150620, 48.20051614449766930, -3.727524721679154940 ) ) ;
#931 = ADVANCED_FACE ( 'NONE', ( #12055 ), #11004, .F. ) ;
#932 = DIRECTION ( 'NONE',  ( -1.000000000000000000, 0.000000000000000000, 0.000000000000000000 ) ) ;
#933 = CARTESIAN_POINT ( 'NONE',  ( 55.94051828345050836, 61.79948385550239465, -4.345558710429104465 ) ) ;
#934 = CARTESIAN_POINT ( 'NONE',  ( 55.96859303347804371, 54.19948385550240033, 4.306917132069425946 ) ) ;
#935 = AXIS2_PLACEMENT_3D ( 'NONE', #208, #4428, #11687 ) ;
#936 = ADVANCED_FACE ( 'NONE', ( #551 ), #3748, .F. ) ;
#937 = ORIENTED_EDGE ( 'NONE', *, *, #11649, .F. ) ;
#938 = CARTESIAN_POINT ( 'NONE',  ( 49.97728705011488159, 53.49948385550240459, -7.000000000000000888 ) ) ;
#939 = VECTOR ( 'NONE', #6527, 999.9999999999998863 ) ;
#940 = VERTEX_POINT ( 'NONE', #3983 ) ;
#941 = EDGE_LOOP ( 'NONE', ( #8309, #9440 ) ) ;
#942 = B_SPLINE_CURVE_WITH_KNOTS ( 'NONE', 3,
 ( #7432, #87, #10669, #977 ),
 .UNSPECIFIED., .F., .F.,
 ( 4, 4 ),
 ( 0.000000000000000000, 0.002080789711329271950 ),
 .UNSPECIFIED. ) ;
#943 = DIRECTION ( 'NONE',  ( -0.000000000000000000, -0.000000000000000000, -1.000000000000000000 ) ) ;
#944 = DIRECTION ( 'NONE',  ( -0.000000000000000000, -0.000000000000000000, -1.000000000000000000 ) ) ;
#945 = LINE ( 'NONE', #10290, #2409 ) ;
#946 = CARTESIAN_POINT ( 'NONE',  ( 55.96859303347802239, 48.80051614449766362, -4.306917132069484566 ) ) ;
#947 = DIRECTION ( 'NONE',  ( -0.8660254037844412611, 0.4999999999999956146, 0.000000000000000000 ) ) ;
#948 = CARTESIAN_POINT ( 'NONE',  ( 42.38452918213188525, 65.09948385550239891, -2.450534656007040013 ) ) ;
#949 = CARTESIAN_POINT ( 'NONE',  ( 42.39856655714566358, 56.89948385550240317, 2.493737253992119207 ) ) ;
#950 = ORIENTED_EDGE ( 'NONE', *, *, #3505, .T. ) ;
#951 = ORIENTED_EDGE ( 'NONE', *, *, #9608, .T. ) ;
#952 = DIRECTION ( 'NONE',  ( -1.000000000000000000, 0.000000000000000000, 0.000000000000000000 ) ) ;
#953 = LINE ( 'NONE', #9544, #6686 ) ;
#954 = CARTESIAN_POINT ( 'NONE',  ( 4.197393957002303999, 0.8151795401431359833, -3.503767560748935139 ) ) ;
#955 = CARTESIAN_POINT ( 'NONE',  ( 6.534838248920897819, 2.951765777552411318, -5.112608298763837489 ) ) ;
#956 = CARTESIAN_POINT ( 'NONE',  ( 44.28664221472221385, 47.90051614449765793, 1.832500667257213722 ) ) ;
#957 = CARTESIAN_POINT ( 'NONE',  ( 44.05948171654945611, 62.20051614449765509, -4.345558710429044069 ) ) ;
#958 = CIRCLE ( 'NONE', #7613, 0.2000000000000000944 ) ;
#959 = CARTESIAN_POINT ( 'NONE',  ( 47.42335538002188144, 46.59948385550239891, 8.007379884777233059 ) ) ;
#960 = ADVANCED_FACE ( 'NONE', ( #13302 ), #10599, .F. ) ;
#961 = MANIFOLD_SOLID_BREP ( 'Cavity1', #5391 ) ;
#962 = DIRECTION ( 'NONE',  ( 0.000000000000000000, 0.000000000000000000, 1.000000000000000000 ) ) ;
#963 = VECTOR ( 'NONE', #11375, 1000.000000000000000 ) ;
#964 = CARTESIAN_POINT ( 'NONE',  ( 52.57664461997821093, 47.40051614449765793, 8.007379884777206414 ) ) ;
#965 = AXIS2_PLACEMENT_3D ( 'NONE', #4001, #12570, #10361 ) ;
#966 = VERTEX_POINT ( 'NONE', #3845 ) ;
#967 = VERTEX_POINT ( 'NONE', #1762 ) ;
#968 = PRODUCT_DEFINITION_CONTEXT ( 'detailed design', #5938, 'design' ) ;
#969 = EDGE_LOOP ( 'NONE', ( #7359, #2872, #11647, #5301 ) ) ;
#970 = VECTOR ( 'NONE', #4699, 1000.000000000000000 ) ;
#971 = CARTESIAN_POINT ( 'NONE',  ( 6.385552186430389021, 5.773502691896261751, 0.000000000000000000 ) ) ;
#972 = CARTESIAN_POINT ( 'NONE',  ( 6.452281807715818829, 2.898928808472990948, -5.021091983800339165 ) ) ;
#973 = DIRECTION ( 'NONE',  ( 0.000000000000000000, 0.000000000000000000, -1.000000000000000000 ) ) ;
#974 = AXIS2_PLACEMENT_3D ( 'NONE', #13105, #9180, #2883 ) ;
#975 = DIRECTION ( 'NONE',  ( -1.000000000000000000, 0.000000000000000000, 0.000000000000000000 ) ) ;
#976 = CARTESIAN_POINT ( 'NONE',  ( 49.97728705011488870, 47.49948385550240459, -6.000000000000000888 ) ) ;
#977 = CARTESIAN_POINT ( 'NONE',  ( 3.973110223767137850, 2.263269463293572928E-11, 3.565797985667434222 ) ) ;
#978 = CARTESIAN_POINT ( 'NONE',  ( 42.63976443033212860, 58.00051614449765225, -0.02388180880514948964 ) ) ;
#979 = FACE_OUTER_BOUND ( 'NONE', #5997, .T. ) ;
#980 = DIRECTION ( 'NONE',  ( 0.000000000000000000, -0.000000000000000000, 1.000000000000000000 ) ) ;
#981 = LINE ( 'NONE', #9300, #11977 ) ;
#982 = CARTESIAN_POINT ( 'NONE',  ( 50.02271294988505446, 52.50051614449765935, -7.000000000000000888 ) ) ;
#983 = CARTESIAN_POINT ( 'NONE',  ( 55.71335778527780747, 56.09948385550240602, 1.832500667257165983 ) ) ;
#984 = DIRECTION ( 'NONE',  ( 1.000000000000000000, 0.000000000000000000, -0.000000000000000000 ) ) ;
#985 = ORIENTED_EDGE ( 'NONE', *, *, #7880, .F. ) ;
#986 = DIRECTION ( 'NONE',  ( 1.000000000000000000, 0.000000000000000000, 0.000000000000000000 ) ) ;
#987 = ORIENTED_EDGE ( 'NONE', *, *, #1362, .T. ) ;
#988 = ORIENTED_EDGE ( 'NONE', *, *, #1729, .F. ) ;
#989 = CARTESIAN_POINT ( 'NONE',  ( 2.100000000000000089, 0.000000000000000000, -5.000000000000000000 ) ) ;
#990 = ADVANCED_FACE ( 'NONE', ( #9245 ), #7176, .T. ) ;
#991 = CARTESIAN_POINT ( 'NONE',  ( -22.00000000000000000, -19.99999999999999289, -20.00000000000000000 ) ) ;
#992 = CARTESIAN_POINT ( 'NONE',  ( 6.212075932873402984, -2.040040303548923628, 4.999999999999999112 ) ) ;
#993 = SURFACE_STYLE_USAGE ( .BOTH. , #2878 ) ;
#994 = DIRECTION ( 'NONE',  ( -0.000000000000000000, 1.000000000000000000, -0.000000000000000000 ) ) ;
#995 = EDGE_CURVE ( 'NONE', #3770, #10955, #495, .T. ) ;
#996 = CARTESIAN_POINT ( 'NONE',  ( 2.449293598294706513E-15, -20.00000000000000000, 9.000000000000000000 ) ) ;
#997 = CARTESIAN_POINT ( 'NONE',  ( 49.97728705011494554, 53.50051614449767357, 6.000000000000000888 ) ) ;
#998 = CARTESIAN_POINT ( 'NONE',  ( -6.165086708099547508, -6.325508935188330462, 9.000000000000000000 ) ) ;
#999 = CARTESIAN_POINT ( 'NONE',  ( 54.13287192849676188, 62.29948385550240886, 5.649768623646098220 ) ) ;
#1000 = CARTESIAN_POINT ( 'NONE',  ( 45.90387839640214196, 60.69948385550240033, 5.676469297603166098 ) ) ;
#1001 = CARTESIAN_POINT ( 'NONE',  ( 52.25172492374522903, 61.59948385550239891, -7.007379884777225953 ) ) ;
#1002 = EDGE_LOOP ( 'NONE', ( #6522, #6191, #11931, #5858 ) ) ;
#1003 = ORIENTED_EDGE ( 'NONE', *, *, #12384, .T. ) ;
#1004 = DIRECTION ( 'NONE',  ( -0.000000000000000000, 1.000000000000000000, -0.000000000000000000 ) ) ;
#1005 = DIRECTION ( 'NONE',  ( 0.000000000000000000, 0.000000000000000000, -1.000000000000000000 ) ) ;
#1006 = CARTESIAN_POINT ( 'NONE',  ( 0.000000000000000000, 0.000000000000000000, -5.000000000000000000 ) ) ;
#1007 = CARTESIAN_POINT ( 'NONE',  ( -20.00000000000000000, -19.99999999999999289, -23.00000000000000000 ) ) ;
#1008 = CARTESIAN_POINT ( 'NONE',  ( 50.02271294988512551, 46.49948385550240459, 7.000000000000000888 ) ) ;
#1009 = VECTOR ( 'NONE', #6135, 1000.000000000000114 ) ;
#1010 = CARTESIAN_POINT ( 'NONE',  ( 45.90387839640208512, 50.30051614449766362, -5.676469297603124353 ) ) ;
#1011 = PRODUCT ( 'motor', 'motor', '', ( #7156 ) ) ;
#1012 = DIRECTION ( 'NONE',  ( -9.858538378746663627E-23, 5.031452844637890958E-23, -1.000000000000000000 ) ) ;
#1013 = ADVANCED_FACE ( 'NONE', ( #3914 ), #6499, .T. ) ;
#1014 = CARTESIAN_POINT ( 'NONE',  ( 45.90387839640214196, 46.69948385550240744, 5.676469297603166098 ) ) ;
#1015 = PRESENTATION_LAYER_ASSIGNMENT (  '', '', ( #3898 ) ) ;
#1016 = PLANE ( 'NONE',  #1563 ) ;
#1017 = CARTESIAN_POINT ( 'NONE',  ( 42.39856655714566358, 58.89948385550241028, 2.493737253992119207 ) ) ;
#1018 = ORIENTED_EDGE ( 'NONE', *, *, #3599, .T. ) ;
#1019 = VERTEX_POINT ( 'NONE', #5356 ) ;
#1020 = CARTESIAN_POINT ( 'NONE',  ( 3.020236159542449172, -23.98474259401938014, -8.999999999999998224 ) ) ;
#1021 = EDGE_CURVE ( 'NONE', #11408, #1099, #7809, .T. ) ;
#1022 = ADVANCED_FACE ( 'NONE', ( #3205 ), #12346, .F. ) ;
#1023 = DIRECTION ( 'NONE',  ( 1.000000000000000000, 0.000000000000000000, 0.000000000000000000 ) ) ;
#1024 = LINE ( 'NONE', #865, #1101 ) ;
#1025 = CARTESIAN_POINT ( 'NONE',  ( -74.99999999999997158, 32.50000000000001421, 15.00000000000000000 ) ) ;
#1026 = CARTESIAN_POINT ( 'NONE',  ( 44.30067958973594955, 50.10051614449766078, -1.875703265242155693 ) ) ;
#1027 = CARTESIAN_POINT ( 'NONE',  ( 45.90387839640208512, 58.30051614449766362, -5.676469297603124353 ) ) ;
#1028 = CARTESIAN_POINT ( 'NONE',  ( 42.39856655714566358, 46.89948385550240317, 2.493737253992119207 ) ) ;
#1029 = MANIFOLD_SOLID_BREP ( 'FlangeHexFillet', #6053 ) ;
#1030 = DIRECTION ( 'NONE',  ( 0.000000000000000000, 0.000000000000000000, 1.000000000000000000 ) ) ;
#1031 = CARTESIAN_POINT ( 'NONE',  ( 45.27934281921082516, 57.70051614449766930, 6.458785618021089192 ) ) ;
#1032 = EDGE_LOOP ( 'NONE', ( #8046, #6869, #12318, #1285 ) ) ;
#1033 = ORIENTED_EDGE ( 'NONE', *, *, #12965, .F. ) ;
#1034 = ORIENTED_EDGE ( 'NONE', *, *, #11991, .F. ) ;
#1035 = CYLINDRICAL_SURFACE ( 'NONE', #7896, 15.00000000000000000 ) ;
#1036 = EDGE_CURVE ( 'NONE', #7994, #9043, #4309, .T. ) ;
#1037 = FACE_OUTER_BOUND ( 'NONE', #7504, .T. ) ;
#1038 = DIRECTION ( 'NONE',  ( 1.000000000000000000, 0.000000000000000000, -0.000000000000000000 ) ) ;
#1039 = CARTESIAN_POINT ( 'NONE',  ( 49.97728705011488870, 51.49948385550240459, -6.000000000000000888 ) ) ;
#1040 = DIRECTION ( 'NONE',  ( -1.000000000000000000, 0.000000000000000000, 0.000000000000000000 ) ) ;
#1041 = CARTESIAN_POINT ( 'NONE',  ( 50.02271294988505446, 46.50051614449766646, -8.000000000000001776 ) ) ;
#1042 = CARTESIAN_POINT ( 'NONE',  ( 2.000000000000000000, 1.773042676681340524, -2.059984127722458425E-15 ) ) ;
#1043 = DIRECTION ( 'NONE',  ( -0.000000000000000000, -0.000000000000000000, 1.000000000000000000 ) ) ;
#1044 = CARTESIAN_POINT ( 'NONE',  ( 0.2499999999999966416, -8.096141056083448362, -1.000000000000000000 ) ) ;
#1045 = CARTESIAN_POINT ( 'NONE',  ( 52.25172492374527877, 55.40051614449764372, 7.007379884777203749 ) ) ;
#1046 = CARTESIAN_POINT ( 'NONE',  ( 46.45491332379572924, 61.29948385550240886, -4.840751629271157874 ) ) ;
#1047 = FACE_OUTER_BOUND ( 'NONE', #2834, .T. ) ;
#1048 = ORIENTED_EDGE ( 'NONE', *, *, #6072, .F. ) ;
#1049 = DIRECTION ( 'NONE',  ( -1.000000000000000000, -0.000000000000000000, -0.000000000000000000 ) ) ;
#1050 = VERTEX_POINT ( 'NONE', #12862 ) ;
#1051 = DIRECTION ( 'NONE',  ( -1.000000000000000000, 0.000000000000000000, 0.000000000000000000 ) ) ;
#1052 = VECTOR ( 'NONE', #6708, 1000.000000000000000 ) ;
#1053 = DIRECTION ( 'NONE',  ( 0.000000000000000000, 0.000000000000000000, 1.000000000000000000 ) ) ;
#1054 =( BOUNDED_SURFACE ( )  B_SPLINE_SURFACE ( 3, 2, ( 
 ( #13175, #7879, #5809 ),
 ( #3788, #1423, #2608 ),
 ( #5738, #10904, #3716 ),
 ( #9044, #2539, #11041 ),
 ( #4629, #5670, #10145 ),
 ( #9939, #5945, #10004 ) ),
 .UNSPECIFIED., .F., .F., .F. ) 
 B_SPLINE_SURFACE_WITH_KNOTS ( ( 4, 2, 4 ),
 ( 3, 3 ),
 ( 0.01652267773200353021, 0.01858309280828997212, 0.02064350788457641403 ),
 ( 0.000000000000000000, 1.000000000000000000 ),
 .UNSPECIFIED. ) 
 GEOMETRIC_REPRESENTATION_ITEM ( )  RATIONAL_B_SPLINE_SURFACE ( (
 ( 1.000000000000000000, 0.8047780975688292315, 1.000000000000000000),
 ( 1.000000000000000000, 0.8123789546324570177, 1.000000000000000000),
 ( 1.000000000000000000, 0.8190677982988761041, 1.000000000000000000),
 ( 1.000000000000000000, 0.8192346069552172150, 1.000000000000000000),
 ( 1.000000000000000000, 0.8126126759768884655, 1.000000000000000000),
 ( 1.000000000000000000, 0.8047712639311999094, 1.000000000000000000) ) ) 
 REPRESENTATION_ITEM ( '' )  SURFACE ( )  );
#1055 = DIRECTION ( 'NONE',  ( 0.000000000000000000, 0.000000000000000000, 1.000000000000000000 ) ) ;
#1056 =( GEOMETRIC_REPRESENTATION_CONTEXT ( 3 ) GLOBAL_UNCERTAINTY_ASSIGNED_CONTEXT ( ( #8827 ) ) GLOBAL_UNIT_ASSIGNED_CONTEXT ( ( #63, #2260, #8567 ) ) REPRESENTATION_CONTEXT ( 'NONE', 'WORKASPACE' ) );
#1057 = FILL_AREA_STYLE ('',( #7645 ) ) ;
#1058 = CARTESIAN_POINT ( 'NONE',  ( 42.63976443033212860, 50.99948385550240459, 0.02388180880522514787 ) ) ;
#1059 = CARTESIAN_POINT ( 'NONE',  ( -0.5469614295416921346, 4.303013824936271270, -3.535263753543735454 ) ) ;
#1060 = CARTESIAN_POINT ( 'NONE',  ( 44.30067958973594955, 52.10051614449766788, -1.875703265242155693 ) ) ;
#1061 = CARTESIAN_POINT ( 'NONE',  ( 2.449293598294706513E-15, -20.00000000000000000, 9.000000000000000000 ) ) ;
#1062 = CARTESIAN_POINT ( 'NONE',  ( 43.33558569842703179, 63.09948385550240602, -2.141517661632099223 ) ) ;
#1063 = CARTESIAN_POINT ( 'NONE',  ( 54.09612160359786515, 61.69948385550240744, -5.676469297603166098 ) ) ;
#1064 = CARTESIAN_POINT ( 'NONE',  ( 45.90387839640214196, 62.69948385550240744, 5.676469297603166098 ) ) ;
#1065 = VERTEX_POINT ( 'NONE', #8795 ) ;
#1066 = CIRCLE ( 'NONE', #4398, 6.080745460913608902 ) ;
#1067 = ORIENTED_EDGE ( 'NONE', *, *, #10529, .F. ) ;
#1068 = CARTESIAN_POINT ( 'NONE',  ( -0.5449313310646672903, -4.304185902836978883, -3.316620875263469159 ) ) ;
#1069 = LINE ( 'NONE', #12828, #12242 ) ;
#1070 = CARTESIAN_POINT ( 'NONE',  ( 4.030867648406620596, -2.329326259789657350, 2.965488570640411492 ) ) ;
#1071 = DIRECTION ( 'NONE',  ( 0.000000000000000000, 1.000000000000000000, 0.000000000000000000 ) ) ;
#1072 = CARTESIAN_POINT ( 'NONE',  ( 44.05948171654949874, 46.79948385550240175, 4.345558710429104465 ) ) ;
#1073 = CARTESIAN_POINT ( 'NONE',  ( 47.70284917648459100, 49.60051614449763946, 6.992620115222796251 ) ) ;
#1074 = DIRECTION ( 'NONE',  ( 0.000000000000000000, 0.000000000000000000, 1.000000000000000000 ) ) ;
#1075 = CARTESIAN_POINT ( 'NONE',  ( 43.33558569842703179, 47.09948385550240602, -2.141517661632099223 ) ) ;
#1076 = SURFACE_STYLE_USAGE ( .BOTH. , #5467 ) ;
#1077 = AXIS2_PLACEMENT_3D ( 'NONE', #3557, #11993, #3627 ) ;
#1078 = CARTESIAN_POINT ( 'NONE',  ( 42.38452918213188525, 59.09948385550240602, -2.450534656007040013 ) ) ;
#1079 = AXIS2_PLACEMENT_3D ( 'NONE', #9191, #11258, #1779 ) ;
#1080 = ADVANCED_FACE ( 'NONE', ( #1308 ), #13067, .F. ) ;
#1081 = ORIENTED_EDGE ( 'NONE', *, *, #7273, .T. ) ;
#1082 = ORIENTED_EDGE ( 'NONE', *, *, #503, .T. ) ;
#1083 = DIRECTION ( 'NONE',  ( 0.000000000000000000, 0.000000000000000000, 1.000000000000000000 ) ) ;
#1084 = CARTESIAN_POINT ( 'NONE',  ( 20.00000000000000000, -14.99999999999999289, -20.00000000000000000 ) ) ;
#1085 = CARTESIAN_POINT ( 'NONE',  ( 6.534838248920899595, -2.951765777552420644, -5.112608298763837489 ) ) ;
#1086 = DIRECTION ( 'NONE',  ( 1.000000000000000000, 0.000000000000000000, 0.000000000000000000 ) ) ;
#1087 = MECHANICAL_DESIGN_GEOMETRIC_PRESENTATION_REPRESENTATION (  '', ( #1966 ), #2431 ) ;
#1088 = AXIS2_PLACEMENT_3D ( 'NONE', #1977, #9515, #7322 ) ;
#1089 = CARTESIAN_POINT ( 'NONE',  ( 48.02776887271750184, 49.60051614449766788, 5.992620115222795363 ) ) ;
#1090 = CARTESIAN_POINT ( 'NONE',  ( 56.66441430157294690, 60.90051614449766504, -2.141517661632166281 ) ) ;
#1091 = EDGE_CURVE ( 'NONE', #5946, #5030, #9628, .T. ) ;
#1092 = CARTESIAN_POINT ( 'NONE',  ( 57.61547081786810764, 62.90051614449765083, -2.450534656007114176 ) ) ;
#1093 = ADVANCED_FACE ( 'NONE', ( #2423 ), #221, .T. ) ;
#1094 = CARTESIAN_POINT ( 'NONE',  ( 4.055492966679600464, 2.385006769472780785, 3.005124364834443451 ) ) ;
#1095 = ADVANCED_FACE ( 'NONE', ( #9833 ), #7627, .T. ) ;
#1096 = CARTESIAN_POINT ( 'NONE',  ( 43.20883090819742023, 58.20051614449766220, -4.963592699178938972 ) ) ;
#1097 = ADVANCED_FACE ( 'NONE', ( #154 ), #12997, .T. ) ;
#1098 = ORIENTED_EDGE ( 'NONE', *, *, #5605, .T. ) ;
#1099 = VERTEX_POINT ( 'NONE', #352 ) ;
#1100 = ORIENTED_EDGE ( 'NONE', *, *, #4158, .F. ) ;
#1101 = VECTOR ( 'NONE', #4222, 1000.000000000000000 ) ;
#1102 = DIRECTION ( 'NONE',  ( -9.858538378746663627E-23, 5.031452844637890958E-23, -1.000000000000000000 ) ) ;
#1103 = PRESENTATION_STYLE_ASSIGNMENT (( #13485 ) ) ;
#1104 = DIRECTION ( 'NONE',  ( 0.000000000000000000, 0.000000000000000000, 1.000000000000000000 ) ) ;
#1105 = CARTESIAN_POINT ( 'NONE',  ( -4.101948962585905356, -2.368261337751088824, -3.681124513963624167 ) ) ;
#1106 = DIRECTION ( 'NONE',  ( -1.000000000000000000, 0.000000000000000000, 0.000000000000000000 ) ) ;
#1107 = CARTESIAN_POINT ( 'NONE',  ( 55.69932041026404335, 47.89948385550240317, -1.875703265242203432 ) ) ;
#1108 = CARTESIAN_POINT ( 'NONE',  ( 50.02271294988512551, 64.49948385550240459, 7.000000000000000888 ) ) ;
#1109 = CARTESIAN_POINT ( 'NONE',  ( 56.81924384183006538, 46.80051614449766362, -4.924951120819380357 ) ) ;
#1110 = VECTOR ( 'NONE', #8764, 1000.000000000000000 ) ;
#1111 = DIRECTION ( 'NONE',  ( 0.000000000000000000, 0.8660254037844380415, -0.5000000000000012212 ) ) ;
#1112 = CARTESIAN_POINT ( 'NONE',  ( 0.000000000000000000, 4.330127018922190985, 2.500000000000005329 ) ) ;
#1113 = CARTESIAN_POINT ( 'NONE',  ( 45.90387839640208512, 60.30051614449766362, -5.676469297603124353 ) ) ;
#1114 = CARTESIAN_POINT ( 'NONE',  ( 48.02776887271745210, 61.39948385550240317, -5.992620115222778487 ) ) ;
#1115 = DIRECTION ( 'NONE',  ( 0.000000000000000000, 1.000000000000000000, 0.000000000000000000 ) ) ;
#1116 = EDGE_CURVE ( 'NONE', #8295, #7686, #2292, .T. ) ;
#1117 = VERTEX_POINT ( 'NONE', #6728 ) ;
#1118 = CARTESIAN_POINT ( 'NONE',  ( 8.500000000000000000, -5.773502691896263528, 0.000000000000000000 ) ) ;
#1119 = ORIENTED_EDGE ( 'NONE', *, *, #325, .F. ) ;
#1120 = FACE_BOUND ( 'NONE', #6057, .T. ) ;
#1121 = AXIS2_PLACEMENT_3D ( 'NONE', #4108, #13625, #12728 ) ;
#1122 = CIRCLE ( 'NONE', #13047, 5.560781378645573980 ) ;
#1123 = DIRECTION ( 'NONE',  ( -0.000000000000000000, -0.000000000000000000, 1.000000000000000000 ) ) ;
#1124 = FACE_OUTER_BOUND ( 'NONE', #456, .T. ) ;
#1125 = DIRECTION ( 'NONE',  ( 0.000000000000000000, 0.000000000000000000, 1.000000000000000000 ) ) ;
#1126 = CARTESIAN_POINT ( 'NONE',  ( 44.03140696652192787, 49.19948385550240033, -4.306917132069425058 ) ) ;
#1127 = CARTESIAN_POINT ( 'NONE',  ( -65.14999999999996305, 32.50000000000001421, -15.00000000000000000 ) ) ;
#1128 = CARTESIAN_POINT ( 'NONE',  ( 43.69122665457040000, 50.00051614449765935, -0.02388180880515696977 ) ) ;
#1129 = CARTESIAN_POINT ( 'NONE',  ( 0.000000000000000000, 3.061616997868383634E-16, -2.500000000000000444 ) ) ;
#1130 = DIRECTION ( 'NONE',  ( 0.8191520442889875797, 0.000000000000000000, 0.5735764363510522656 ) ) ;
#1131 = ADVANCED_FACE ( 'NONE', ( #1446, #2354, #4579 ), #1377, .F. ) ;
#1132 = CARTESIAN_POINT ( 'NONE',  ( 52.25172492374522903, 59.59948385550240602, -7.007379884777225953 ) ) ;
#1133 = CIRCLE ( 'NONE', #4918, 1.535500000000000087 ) ;
#1134 = FACE_BOUND ( 'NONE', #8492, .T. ) ;
#1135 = EDGE_CURVE ( 'NONE', #11879, #2319, #10522, .T. ) ;
#1136 = VECTOR ( 'NONE', #2029, 1000.000000000000000 ) ;
#1137 = CONICAL_SURFACE ( 'NONE', #8884, 2.059999999999998721, 0.9599310885968738161 ) ;
#1138 = B_SPLINE_CURVE_WITH_KNOTS ( 'NONE', 3,
 ( #9599, #1271, #123, #10701, #2058, #12700, #3371, #7460 ),
 .UNSPECIFIED., .F., .F.,
 ( 4, 2, 2, 4 ),
 ( 2.465131517071352357E-07, 0.001183067374689843057, 0.001774477805458910071, 0.002365888236227977302 ),
 .UNSPECIFIED. ) ;
#1139 = ORIENTED_EDGE ( 'NONE', *, *, #8132, .T. ) ;
#1140 = ORIENTED_EDGE ( 'NONE', *, *, #3820, .F. ) ;
#1141 = ORIENTED_EDGE ( 'NONE', *, *, #6219, .T. ) ;
#1142 = CARTESIAN_POINT ( 'NONE',  ( 4.175075985190098038, 4.120741555260245548, 3.964526709274768569E-16 ) ) ;
#1143 = CARTESIAN_POINT ( 'NONE',  ( 6.534838248920897819, 2.951765777552411318, -5.112608298763837489 ) ) ;
#1144 = DIRECTION ( 'NONE',  ( 0.000000000000000000, 0.000000000000000000, 1.000000000000000000 ) ) ;
#1145 = AXIS2_PLACEMENT_3D ( 'NONE', #11029, #10129, #4890 ) ;
#1146 = DIRECTION ( 'NONE',  ( 1.000000000000000000, 0.000000000000000000, 0.000000000000000000 ) ) ;
#1147 = CARTESIAN_POINT ( 'NONE',  ( 56.65037692655918988, 53.89948385550240317, -2.184720259617163762 ) ) ;
#1148 = APPLICATION_CONTEXT ( 'automotive_design' ) ;
#1149 = CIRCLE ( 'NONE', #9121, 15.00000000000000000 ) ;
#1150 = CARTESIAN_POINT ( 'NONE',  ( 52.29715082351538769, 44.60051614449766788, -6.992620115222796251 ) ) ;
#1151 = DIRECTION ( 'NONE',  ( 0.000000000000000000, 0.000000000000000000, 1.000000000000000000 ) ) ;
#1152 = CARTESIAN_POINT ( 'NONE',  ( 47.37792948025162332, 63.39948385550238896, -7.992620115222770494 ) ) ;
#1153 = DIRECTION ( 'NONE',  ( 0.000000000000000000, 0.000000000000000000, 1.000000000000000000 ) ) ;
#1154 = CARTESIAN_POINT ( 'NONE',  ( 45.31609314410967926, 58.69948385550240033, 6.485486291978119766 ) ) ;
#1155 = ORIENTED_EDGE ( 'NONE', *, *, #6325, .F. ) ;
#1156 = VECTOR ( 'NONE', #12886, 1000.000000000000000 ) ;
#1157 = ORIENTED_EDGE ( 'NONE', *, *, #10798, .T. ) ;
#1158 = EDGE_CURVE ( 'NONE', #8508, #7078, #7834, .T. ) ;
#1159 = LINE ( 'NONE', #4355, #7189 ) ;
#1160 = B_SPLINE_CURVE_WITH_KNOTS ( 'NONE', 3,
 ( #4393, #3360, #9652, #6425, #175, #11791, #6614, #7584, #12749, #112, #7453, #3293, #1260, #9787, #8755, #7720 ),
 .UNSPECIFIED., .F., .F.,
 ( 4, 3, 3, 3, 3, 4 ),
 ( -2.669610558405663348E-06, 0.000000000000000000, 5.703179328867284594E-05, 0.0001157653700806020010, 0.0001686517580799737359, 0.0002219032271235107196 ),
 .UNSPECIFIED. ) ;
#1161 = DIRECTION ( 'NONE',  ( 0.000000000000000000, 0.000000000000000000, 1.000000000000000000 ) ) ;
#1162 = COLOUR_RGB ( '',1.000000000000000000, 0.9490196078431372140, 0.9098039215686274384 ) ;
#1163 = DIRECTION ( 'NONE',  ( 1.000000000000000000, 0.000000000000000000, 0.000000000000000000 ) ) ;
#1164 = CARTESIAN_POINT ( 'NONE',  ( 48.07319477248762496, 48.40051614449766504, -6.007379884777208190 ) ) ;
#1165 = CARTESIAN_POINT ( 'NONE',  ( 45.86712807150329496, 61.70051614449766220, 5.649768623646139964 ) ) ;
#1166 = CARTESIAN_POINT ( 'NONE',  ( 47.37792948025162332, 47.39948385550241028, -7.992620115222770494 ) ) ;
#1167 = LINE ( 'NONE', #8721, #8679 ) ;
#1168 = CARTESIAN_POINT ( 'NONE',  ( 50.02271294988505446, 58.50051614449765225, -8.000000000000001776 ) ) ;
#1169 = ORIENTED_EDGE ( 'NONE', *, *, #5857, .F. ) ;
#1170 = ORIENTED_EDGE ( 'NONE', *, *, #7701, .F. ) ;
#1171 = VERTEX_POINT ( 'NONE', #8736 ) ;
#1172 = DIRECTION ( 'NONE',  ( 0.000000000000000000, 1.000000000000000000, 0.000000000000000000 ) ) ;
#1173 = CARTESIAN_POINT ( 'NONE',  ( 6.466260427357672924, 2.904280683598007951, -5.030361703432632225 ) ) ;
#1175 = VECTOR ( 'NONE', #104, 1000.000000000000000 ) ;
#1174 = DIRECTION ( 'NONE',  ( 1.000000000000000000, 0.000000000000000000, 0.000000000000000000 ) ) ;
#1176 = FACE_OUTER_BOUND ( 'NONE', #1752, .T. ) ;
#1177 = SURFACE_STYLE_USAGE ( .BOTH. , #12280 ) ;
#1178 = CARTESIAN_POINT ( 'NONE',  ( 44.28664221472220675, 47.09948385550240602, -1.832500667257165317 ) ) ;
#1179 = CARTESIAN_POINT ( 'NONE',  ( 50.02271294988512551, 62.49948385550240459, 7.000000000000000888 ) ) ;
#1180 = CARTESIAN_POINT ( 'NONE',  ( 49.97728705011495265, 45.50051614449766646, 8.000000000000001776 ) ) ;
#1181 = LINE ( 'NONE', #1042, #8228 ) ;
#1182 = CARTESIAN_POINT ( 'NONE',  ( -17.85000000000000142, -19.99999999999999289, -20.00000000000000000 ) ) ;
#1183 = CARTESIAN_POINT ( 'NONE',  ( 47.70284917648459100, 55.60051614449764656, 6.992620115222796251 ) ) ;
#1184 = CARTESIAN_POINT ( 'NONE',  ( 44.30067958973596376, 60.89948385550241028, 1.875703265242204099 ) ) ;
#1185 = CONICAL_SURFACE ( 'NONE', #3190, 1.610000000000000098, 0.7853981633974658205 ) ;
#1186 = ORIENTED_EDGE ( 'NONE', *, *, #10636, .T. ) ;
#1187 = MANIFOLD_SOLID_BREP ( 'Hex', #8467 ) ;
#1188 = DIRECTION ( 'NONE',  ( -3.469446951953614682E-16, 1.000000000000000000, 0.000000000000000000 ) ) ;
#1189 = VECTOR ( 'NONE', #11314, 1000.000000000000000 ) ;
#1190 = EDGE_LOOP ( 'NONE', ( #2623, #5170, #4957, #13127 ) ) ;
#1191 = CARTESIAN_POINT ( 'NONE',  ( -2.852594293689151105E-15, 3.375361811986501426, -1.153701847711632311 ) ) ;
#1192 = DIRECTION ( 'NONE',  ( 1.000000000000000000, 0.000000000000000000, 0.000000000000000000 ) ) ;
#1193 = VECTOR ( 'NONE', #7398, 1000.000000000000000 ) ;
#1194 = CARTESIAN_POINT ( 'NONE',  ( -4.000000000000000000, 0.000000000000000000, 0.000000000000000000 ) ) ;
#1195 = ADVANCED_FACE ( 'NONE', ( #2914 ), #12926, .T. ) ;
#1196 = EDGE_CURVE ( 'NONE', #4847, #8976, #4787, .T. ) ;
#1197 = CARTESIAN_POINT ( 'NONE',  ( 0.000000000000000000, 0.000000000000000000, 0.000000000000000000 ) ) ;
#1198 = CARTESIAN_POINT ( 'NONE',  ( 44.05948171654949874, 50.79948385550238754, 4.345558710429105354 ) ) ;
#1199 = AXIS2_PLACEMENT_3D ( 'NONE', #9457, #9400, #13594 ) ;
#1200 = EDGE_CURVE ( 'NONE', #13024, #10854, #10028, .T. ) ;
#1201 = FACE_OUTER_BOUND ( 'NONE', #4084, .T. ) ;
#1202 = CARTESIAN_POINT ( 'NONE',  ( 43.69122665457040000, 52.00051614449766646, -0.02388180880515696977 ) ) ;
#1203 = CARTESIAN_POINT ( 'NONE',  ( 20.00000000000000000, -25.00000000000000711, -23.00000000000000000 ) ) ;
#1204 = DIRECTION ( 'NONE',  ( -0.000000000000000000, -0.000000000000000000, -1.000000000000000000 ) ) ;
#1205 = SURFACE_STYLE_USAGE ( .BOTH. , #2177 ) ;
#1206 = CARTESIAN_POINT ( 'NONE',  ( 50.02271294988512551, 58.49948385550241170, 7.000000000000000888 ) ) ;
#1207 = CARTESIAN_POINT ( 'NONE',  ( 2.354826896168714434, -6.962563485461402024, -1.000000000000000000 ) ) ;
#1208 = ORIENTED_EDGE ( 'NONE', *, *, #8540, .F. ) ;
#1209 = EDGE_LOOP ( 'NONE', ( #4886, #9308, #8557, #1048 ) ) ;
#1210 = CIRCLE ( 'NONE', #4730, 12.49999999999999645 ) ;
#1211 = VERTEX_POINT ( 'NONE', #1724 ) ;
#1212 = CARTESIAN_POINT ( 'NONE',  ( 4.165266963751722784, 4.099263933823986683, 2.067493599750144616E-15 ) ) ;
#1213 = CARTESIAN_POINT ( 'NONE',  ( 2.449848172108560096, 3.432307619358740514, -3.503702292528905637 ) ) ;
#1214 = CARTESIAN_POINT ( 'NONE',  ( 0.000000000000000000, 0.000000000000000000, -10.00000000000000000 ) ) ;
#1215 = CARTESIAN_POINT ( 'NONE',  ( 2.000000000000000000, 0.8865213383406680414, -1.535500000000000975 ) ) ;
#1216 = CARTESIAN_POINT ( 'NONE',  ( 47.70284917648453415, 55.39948385550239607, -6.992620115222774047 ) ) ;
#1217 = CARTESIAN_POINT ( 'NONE',  ( 47.70284917648459100, 55.60051614449764656, 6.992620115222796251 ) ) ;
#1218 = DIRECTION ( 'NONE',  ( 1.000000000000000000, 3.469446951953615175E-16, 0.000000000000000000 ) ) ;
#1219 = CARTESIAN_POINT ( 'NONE',  ( 56.66441430157296821, 46.09948385550240602, 2.141517661632100111 ) ) ;
#1220 = EDGE_CURVE ( 'NONE', #12388, #4959, #11203, .T. ) ;
#1221 = CARTESIAN_POINT ( 'NONE',  ( 42.38452918213188525, 57.09948385550240602, -2.450534656007040013 ) ) ;
#1222 = ORIENTED_EDGE ( 'NONE', *, *, #8044, .T. ) ;
#1223 = VERTEX_POINT ( 'NONE', #5831 ) ;
#1224 = DIRECTION ( 'NONE',  ( -1.000000000000000000, -0.000000000000000000, -0.000000000000000000 ) ) ;
#1225 = CIRCLE ( 'NONE', #10946, 3.500000000000000000 ) ;
#1226 = EDGE_CURVE ( 'NONE', #11270, #10506, #4928, .T. ) ;
#1227 = PLANE ( 'NONE',  #1317 ) ;
#1228 = CARTESIAN_POINT ( 'NONE',  ( 44.91013252490150620, 46.20051614449766220, -3.727524721679154940 ) ) ;
#1229 = CARTESIAN_POINT ( 'NONE',  ( 50.02271294988505446, 64.50051614449765225, -7.000000000000000888 ) ) ;
#1230 = CARTESIAN_POINT ( 'NONE',  ( 49.97728705011486738, 47.49948385550240459, -8.000000000000001776 ) ) ;
#1231 = CARTESIAN_POINT ( 'NONE',  ( 52.62207051974829852, 56.60051614449765367, -7.992620115222797139 ) ) ;
#1232 = ORIENTED_EDGE ( 'NONE', *, *, #1226, .T. ) ;
#1233 = ORIENTED_EDGE ( 'NONE', *, *, #3769, .T. ) ;
#1234 = ORIENTED_EDGE ( 'NONE', *, *, #13277, .T. ) ;
#1235 = EDGE_LOOP ( 'NONE', ( #3787, #8273, #4869 ) ) ;
#1236 = CYLINDRICAL_SURFACE ( 'NONE', #7578, 4.000000000000003553 ) ;
#1237 = DIRECTION ( 'NONE',  ( 0.000000000000000000, -1.000000000000000000, 0.000000000000000000 ) ) ;
#1238 = CARTESIAN_POINT ( 'NONE',  ( -9.999999999999994671, 20.00000000000001421, 15.00000000000000000 ) ) ;
#1239 = SURFACE_STYLE_USAGE ( .BOTH. , #11768 ) ;
#1240 = CARTESIAN_POINT ( 'NONE',  ( 55.11794222512601493, 52.19948385550240744, 3.688883143319541702 ) ) ;
#1241 = CARTESIAN_POINT ( 'NONE',  ( 43.33558569842703179, 65.09948385550239891, -2.141517661632099223 ) ) ;
#1242 = CARTESIAN_POINT ( 'NONE',  ( 43.18075615816994173, 47.80051614449764941, 4.924951120819380357 ) ) ;
#1243 = DIRECTION ( 'NONE',  ( 1.000000000000000000, 0.000000000000000000, 0.000000000000000000 ) ) ;
#1244 = CARTESIAN_POINT ( 'NONE',  ( 0.3106000600989293203, 5.537975084925940372, 0.4079457818577097994 ) ) ;
#1245 = CARTESIAN_POINT ( 'NONE',  ( 47.74827507625469281, 58.40051614449766504, -7.007379884777203749 ) ) ;
#1246 = CARTESIAN_POINT ( 'NONE',  ( 55.08986747509847248, 55.79948385550239465, -3.727524721679197572 ) ) ;
#1247 = EDGE_LOOP ( 'NONE', ( #12529, #10799, #10589, #5654, #761, #4432 ) ) ;
#1248 = CARTESIAN_POINT ( 'NONE',  ( 1.219878473194463187, -24.84890673354692936, 9.999999999999998224 ) ) ;
#1249 = ORIENTED_EDGE ( 'NONE', *, *, #9161, .F. ) ;
#1250 = LINE ( 'NONE', #6287, #3951 ) ;
#1251 = DIRECTION ( 'NONE',  ( -0.2439756946365075896, 0.9697813467099856144, 1.610118993450814692E-22 ) ) ;
#1252 = CARTESIAN_POINT ( 'NONE',  ( 4.175572532730929431, 2.061029303918044064, -3.569807470274393602 ) ) ;
#1253 = CARTESIAN_POINT ( 'NONE',  ( 49.97728705011488159, 49.49948385550240459, -7.000000000000000888 ) ) ;
#1254 = AXIS2_PLACEMENT_3D ( 'NONE', #12307, #7961, #7061 ) ;
#1255 = CARTESIAN_POINT ( 'NONE',  ( 2.000000000000000000, 1.773042676681340524, -2.059984127722458425E-15 ) ) ;
#1256 = CARTESIAN_POINT ( 'NONE',  ( 56.30877334542961421, 49.00051614449765935, 0.02388180880515774693 ) ) ;
#1257 = ADVANCED_FACE ( 'NONE', ( #12380 ), #8937, .T. ) ;
#1258 = DIRECTION ( 'NONE',  ( 1.000000000000000000, 0.000000000000000000, 0.000000000000000000 ) ) ;
#1259 = CARTESIAN_POINT ( 'NONE',  ( 3.349226789952652439, 2.685125164760731487, -0.2236248678334773199 ) ) ;
#1260 = CARTESIAN_POINT ( 'NONE',  ( 6.420058897733094128, -5.782965130189196223, 5.134498127650324400E-16 ) ) ;
#1261 = CARTESIAN_POINT ( 'NONE',  ( 43.34962307344081012, 58.89948385550241028, 2.184720259617164650 ) ) ;
#1262 = DIRECTION ( 'NONE',  ( 0.000000000000000000, 0.000000000000000000, 1.000000000000000000 ) ) ;
#1263 = ADVANCED_FACE ( 'NONE', ( #7900 ), #147, .T. ) ;
#1264 = EDGE_LOOP ( 'NONE', ( #3888, #6058, #2553, #520 ) ) ;
#1265 = EDGE_CURVE ( 'NONE', #3640, #5736, #4961, .T. ) ;
#1266 = EDGE_CURVE ( 'NONE', #9956, #9726, #6857, .T. ) ;
#1267 = AXIS2_PLACEMENT_3D ( 'NONE', #2661, #378, #508 ) ;
#1268 = ORIENTED_EDGE ( 'NONE', *, *, #11850, .T. ) ;
#1269 = CARTESIAN_POINT ( 'NONE',  ( -4.175002511812151873, -2.208363329454905877, -3.469254087858246738 ) ) ;
#1270 = DIRECTION ( 'NONE',  ( 0.000000000000000000, 0.000000000000000000, 1.000000000000000000 ) ) ;
#1271 = CARTESIAN_POINT ( 'NONE',  ( -3.680118525130244400, 2.494084732383327285, -0.3507732604232449702 ) ) ;
#1272 = EDGE_CURVE ( 'NONE', #4573, #7186, #10236, .T. ) ;
#1273 = FILL_AREA_STYLE_COLOUR ( '', #1315 ) ;
#1274 = CARTESIAN_POINT ( 'NONE',  ( 30.00000000000000355, -40.00000000000000000, 10.00000000000000000 ) ) ;
#1275 = CARTESIAN_POINT ( 'NONE',  ( 47.70284917648453415, 53.39948385550239607, -6.992620115222774047 ) ) ;
#1276 = B_SPLINE_CURVE_WITH_KNOTS ( 'NONE', 3,
 ( #9913, #434, #12128, #2653, #4667, #8890 ),
 .UNSPECIFIED., .F., .F.,
 ( 4, 2, 4 ),
 ( 9.961792871202292917E-20, 0.002086519881787258883, 0.004173039763574517766 ),
 .UNSPECIFIED. ) ;
#1277 = CARTESIAN_POINT ( 'NONE',  ( 54.13287192849671214, 54.70051614449766220, -5.649768623646139964 ) ) ;
#1278 = VECTOR ( 'NONE', #10202, 1000.000000000000000 ) ;
#1279 = CARTESIAN_POINT ( 'NONE',  ( 10.00000000000000000, 25.00000000000001776, 15.00000000000000000 ) ) ;
#1280 = CARTESIAN_POINT ( 'NONE',  ( 45.90387839640214196, 52.69948385550240033, 5.676469297603166098 ) ) ;
#1281 = AXIS2_PLACEMENT_3D ( 'NONE', #8689, #11723, #10814 ) ;
#1282 = DIRECTION ( 'NONE',  ( 0.8660254037844381525, 0.5000000000000009992, 0.000000000000000000 ) ) ;
#1283 = EDGE_CURVE ( 'NONE', #10723, #6266, #543, .T. ) ;
#1284 = CARTESIAN_POINT ( 'NONE',  ( 42.39856655714566358, 64.89948385550239607, 2.493737253992119207 ) ) ;
#1285 = ORIENTED_EDGE ( 'NONE', *, *, #3067, .F. ) ;
#1286 =( GEOMETRIC_REPRESENTATION_CONTEXT ( 3 ) GLOBAL_UNCERTAINTY_ASSIGNED_CONTEXT ( ( #9793 ) ) GLOBAL_UNIT_ASSIGNED_CONTEXT ( ( #8209, #4056, #2043 ) ) REPRESENTATION_CONTEXT ( 'NONE', 'WORKASPACE' ) );
#1287 = ORIENTED_EDGE ( 'NONE', *, *, #1283, .F. ) ;
#1288 = AXIS2_PLACEMENT_3D ( 'NONE', #11344, #5061, #6175 ) ;
#1289 = DIRECTION ( 'NONE',  ( -1.000000000000000000, 1.110223024625156935E-15, 0.000000000000000000 ) ) ;
#1290 = VECTOR ( 'NONE', #1188, 1000.000000000000000 ) ;
#1291 = FACE_BOUND ( 'NONE', #2165, .T. ) ;
#1292 = CARTESIAN_POINT ( 'NONE',  ( 55.08986747509849380, 53.20051614449766220, 3.727524721679155384 ) ) ;
#1293 = CARTESIAN_POINT ( 'NONE',  ( 5.000000000000003553, -20.00000000000000000, -20.00000000000000000 ) ) ;
#1294 = AXIS2_PLACEMENT_3D ( 'NONE', #1197, #9909, #13210 ) ;
#1295 = CARTESIAN_POINT ( 'NONE',  ( 42.39856655714566358, 50.89948385550240317, 2.493737253992119207 ) ) ;
#1296 = AXIS2_PLACEMENT_3D ( 'NONE', #6982, #3932, #10153 ) ;
#1297 = CARTESIAN_POINT ( 'NONE',  ( 52.29715082351547295, 54.39948385550239607, 6.992620115222774047 ) ) ;
#1298 = DIRECTION ( 'NONE',  ( 0.000000000000000000, 0.5000000000000009992, -0.8660254037844380415 ) ) ;
#1299 = CARTESIAN_POINT ( 'NONE',  ( 43.18075615816994173, 55.80051614449766362, 4.924951120819380357 ) ) ;
#1300 = EDGE_CURVE ( 'NONE', #1171, #6264, #7965, .T. ) ;
#1301 = CIRCLE ( 'NONE', #13223, 5.000000000000007994 ) ;
#1302 = VERTEX_POINT ( 'NONE', #6927 ) ;
#1303 = ORIENTED_EDGE ( 'NONE', *, *, #5017, .T. ) ;
#1304 = VERTEX_POINT ( 'NONE', #3947 ) ;
#1305 = ORIENTED_EDGE ( 'NONE', *, *, #10213, .F. ) ;
#1306 = CARTESIAN_POINT ( 'NONE',  ( 1.267864665261691752E-11, -20.00000000000000000, 9.999999999999998224 ) ) ;
#1307 = FACE_OUTER_BOUND ( 'NONE', #8603, .T. ) ;
#1308 = FACE_OUTER_BOUND ( 'NONE', #9255, .T. ) ;
#1309 = CARTESIAN_POINT ( 'NONE',  ( 51.92680522751233951, 53.59948385550240602, -6.007379884777223289 ) ) ;
#1310 = CARTESIAN_POINT ( 'NONE',  ( 42.63976443033212149, 46.00051614449765225, -0.02388180880514948964 ) ) ;
#1311 = CARTESIAN_POINT ( 'NONE',  ( 47.42335538002180328, 46.40051614449765793, -8.007379884777206414 ) ) ;
#1312 = CYLINDRICAL_SURFACE ( 'NONE', #5790, 15.00000000000000000 ) ;
#1313 = PLANE ( 'NONE',  #8899 ) ;
#1314 = CARTESIAN_POINT ( 'NONE',  ( 52.29715082351538769, 58.60051614449766078, -6.992620115222796251 ) ) ;
#1315 = COLOUR_RGB ( '',0.8941176470588234615, 0.8941176470588234615, 0.8941176470588234615 ) ;
#1316 = CARTESIAN_POINT ( 'NONE',  ( 48.07319477248768180, 62.59948385550238470, 6.007379884777225953 ) ) ;
#1317 = AXIS2_PLACEMENT_3D ( 'NONE', #5473, #1427, #6575 ) ;
#1318 = ORIENTED_EDGE ( 'NONE', *, *, #928, .T. ) ;
#1319 = DIRECTION ( 'NONE',  ( 0.03086419753086420623, -0.9995235871707959241, 0.000000000000000000 ) ) ;
#1320 = VERTEX_POINT ( 'NONE', #9211 ) ;
#1321 = DIRECTION ( 'NONE',  ( 0.000000000000000000, 0.000000000000000000, -1.000000000000000000 ) ) ;
#1322 = DIRECTION ( 'NONE',  ( 0.000000000000000000, 0.000000000000000000, -1.000000000000000000 ) ) ;
#1323 = EDGE_CURVE ( 'NONE', #11747, #7759, #358, .T. ) ;
#1324 = CARTESIAN_POINT ( 'NONE',  ( -17.85000000000000142, -19.99999999999999289, -23.00000000000000000 ) ) ;
#1325 = CARTESIAN_POINT ( 'NONE',  ( 44.03140696652192787, 51.19948385550238612, -4.306917132069425058 ) ) ;
#1326 = CYLINDRICAL_SURFACE ( 'NONE', #6419, 4.000000000000000000 ) ;
#1327 = CARTESIAN_POINT ( 'NONE',  ( 43.69122665457040000, 58.00051614449765935, -0.02388180880515696977 ) ) ;
#1328 = EDGE_CURVE ( 'NONE', #11270, #8976, #8325, .T. ) ;
#1329 = DIRECTION ( 'NONE',  ( 0.000000000000000000, 0.000000000000000000, 1.000000000000000000 ) ) ;
#1330 = CARTESIAN_POINT ( 'NONE',  ( -2.595115354961444076, -7.673029147243174641, -1.000000000000000000 ) ) ;
#1331 = CARTESIAN_POINT ( 'NONE',  ( 4.200000000000001954, 0.000000000000000000, 0.000000000000000000 ) ) ;
#1332 = CARTESIAN_POINT ( 'NONE',  ( 48.02776887271745210, 47.39948385550241028, -5.992620115222778487 ) ) ;
#1333 = CARTESIAN_POINT ( 'NONE',  ( 4.211140560182196957, -2.431303136016555122, -3.745885042887436622 ) ) ;
#1334 = ORIENTED_EDGE ( 'NONE', *, *, #4336, .T. ) ;
#1335 = VECTOR ( 'NONE', #1410, 1000.000000000000000 ) ;
#1336 = ORIENTED_EDGE ( 'NONE', *, *, #4161, .T. ) ;
#1337 = DIRECTION ( 'NONE',  ( -1.000000000000000000, 0.000000000000000000, 0.000000000000000000 ) ) ;
#1338 = ADVANCED_FACE ( 'NONE', ( #2777 ), #4067, .F. ) ;
#1339 = CARTESIAN_POINT ( 'NONE',  ( 0.08165819712376803929, -3.720292241887084295, 3.556264818047238041 ) ) ;
#1340 = CARTESIAN_POINT ( 'NONE',  ( 7.500000000000003553, -20.00000000000000000, -10.00000000000000000 ) ) ;
#1341 = PRESENTATION_STYLE_ASSIGNMENT (( #11485 ) ) ;
#1342 = DIRECTION ( 'NONE',  ( -1.000000000000000000, 0.000000000000000000, 0.000000000000000000 ) ) ;
#1343 = CARTESIAN_POINT ( 'NONE',  ( 4.211140560182196957, 2.431303136016536470, -3.745885042887433514 ) ) ;
#1344 = EDGE_CURVE ( 'NONE', #9289, #5152, #12504, .T. ) ;
#1345 = CARTESIAN_POINT ( 'NONE',  ( 57.36023556966787851, 51.99948385550239749, -0.02388180880522424582 ) ) ;
#1346 = AXIS2_PLACEMENT_3D ( 'NONE', #5985, #5016, #6127 ) ;
#1347 = CARTESIAN_POINT ( 'NONE',  ( 43.33558569842706021, 55.90051614449765793, 2.141517661632167169 ) ) ;
#1348 = EDGE_CURVE ( 'NONE', #11125, #10197, #10580, .T. ) ;
#1349 = CARTESIAN_POINT ( 'NONE',  ( -20.00000000000000000, -19.99999999999999289, -12.00000000000000000 ) ) ;
#1350 = MECHANICAL_DESIGN_GEOMETRIC_PRESENTATION_REPRESENTATION (  '', ( #8874 ), #12185 ) ;
#1351 = AXIS2_PLACEMENT_3D ( 'NONE', #7867, #10130, #382 ) ;
#1352 = CARTESIAN_POINT ( 'NONE',  ( 42.63976443033212860, 52.99948385550240459, 0.02388180880522514787 ) ) ;
#1353 = CARTESIAN_POINT ( 'NONE',  ( 2.449293598294706513E-15, -20.00000000000000000, 9.000000000000000000 ) ) ;
#1354 = CARTESIAN_POINT ( 'NONE',  ( 47.37792948025162332, 65.39948385550239607, -7.992620115222770494 ) ) ;
#1355 = EDGE_LOOP ( 'NONE', ( #6215, #4217, #7502, #11183 ) ) ;
#1356 = ORIENTED_EDGE ( 'NONE', *, *, #8047, .T. ) ;
#1357 = CIRCLE ( 'NONE', #4686, 2.149999999999999023 ) ;
#1358 = ORIENTED_EDGE ( 'NONE', *, *, #8589, .T. ) ;
#1359 = CARTESIAN_POINT ( 'NONE',  ( 3.806834918298646731, 3.031088913245537864, 1.750000000000000666 ) ) ;
#1360 = DIRECTION ( 'NONE',  ( -0.7779254092217071648, -0.6283566325640553840, 0.000000000000000000 ) ) ;
#1361 = CARTESIAN_POINT ( 'NONE',  ( 48.07319477248762496, 52.40051614449767214, -6.007379884777208190 ) ) ;
#1362 = EDGE_CURVE ( 'NONE', #11343, #10542, #12586, .T. ) ;
#1363 = CARTESIAN_POINT ( 'NONE',  ( -65.14999999999996305, 32.50000000000001421, 15.00000000000000178 ) ) ;
#1364 = CARTESIAN_POINT ( 'NONE',  ( 47.37792948025162332, 55.39948385550240317, -7.992620115222770494 ) ) ;
#1365 = CARTESIAN_POINT ( 'NONE',  ( 56.66441430157296821, 56.09948385550240602, 2.141517661632100111 ) ) ;
#1366 = PLANE ( 'NONE',  #3601 ) ;
#1367 = CARTESIAN_POINT ( 'NONE',  ( 42.38452918213190657, 63.90051614449765793, 2.450534656007115508 ) ) ;
#1368 = AXIS2_PLACEMENT_3D ( 'NONE', #11641, #2226, #6470 ) ;
#1369 = VERTEX_POINT ( 'NONE', #9546 ) ;
#1370 = ORIENTED_EDGE ( 'NONE', *, *, #840, .F. ) ;
#1371 = ORIENTED_EDGE ( 'NONE', *, *, #6219, .F. ) ;
#1372 = ORIENTED_EDGE ( 'NONE', *, *, #11964, .F. ) ;
#1373 = FACE_OUTER_BOUND ( 'NONE', #11761, .T. ) ;
#1374 = SURFACE_STYLE_USAGE ( .BOTH. , #3334 ) ;
#1375 =( NAMED_UNIT ( * ) PLANE_ANGLE_UNIT ( ) SI_UNIT ( $, .RADIAN. ) );
#1376 = LINE ( 'NONE', #1238, #2906 ) ;
#1377 = PLANE ( 'NONE',  #6559 ) ;
#1378 = CARTESIAN_POINT ( 'NONE',  ( 46.49166364869460466, 58.69948385550240033, 4.867452303228209765 ) ) ;
#1379 = CARTESIAN_POINT ( 'NONE',  ( 52.25172492374528588, 45.40051614449766504, 7.007379884777204637 ) ) ;
#1380 = CARTESIAN_POINT ( 'NONE',  ( 52.62207051974829852, 50.60051614449765367, -7.992620115222797139 ) ) ;
#1381 = PLANE ( 'NONE',  #4015 ) ;
#1382 = DIRECTION ( 'NONE',  ( -0.000000000000000000, -0.000000000000000000, 1.000000000000000000 ) ) ;
#1383 = CARTESIAN_POINT ( 'NONE',  ( 45.27934281921082516, 45.70051614449766220, 6.458785618021089192 ) ) ;
#1384 = VERTEX_POINT ( 'NONE', #10512 ) ;
#1385 = DIRECTION ( 'NONE',  ( 1.000000000000000000, -1.734723475976807341E-16, -0.000000000000000000 ) ) ;
#1386 = VERTEX_POINT ( 'NONE', #1025 ) ;
#1387 = CARTESIAN_POINT ( 'NONE',  ( -6.315157543962389260E-16, -3.838309248099061044, -3.351853367130940065 ) ) ;
#1388 = CARTESIAN_POINT ( 'NONE',  ( 2.899426713160750069, -23.82535289025860337, -9.999999999999994671 ) ) ;
#1389 = CARTESIAN_POINT ( 'NONE',  ( 6.165086708099646984, -33.67449106481162602, 0.000000000000000000 ) ) ;
#1390 = PRODUCT_CONTEXT ( 'NONE', #3103, 'mechanical' ) ;
#1391 = CARTESIAN_POINT ( 'NONE',  ( 47.70284917648453415, 55.39948385550238896, -6.992620115222774047 ) ) ;
#1392 = DIRECTION ( 'NONE',  ( 0.000000000000000000, 0.000000000000000000, -1.000000000000000000 ) ) ;
#1393 = CARTESIAN_POINT ( 'NONE',  ( 53.50833635130544508, 55.30051614449765651, 4.867452303228181343 ) ) ;
#1394 = AXIS2_PLACEMENT_3D ( 'NONE', #5354, #11635, #6333 ) ;
#1395 = PLANE ( 'NONE',  #11068 ) ;
#1396 = DIRECTION ( 'NONE',  ( 0.000000000000000000, 0.000000000000000000, -1.000000000000000000 ) ) ;
#1397 =( NAMED_UNIT ( * ) SI_UNIT ( $, .STERADIAN. ) SOLID_ANGLE_UNIT ( ) );
#1398 = CARTESIAN_POINT ( 'NONE',  ( 52.29715082351547295, 64.39948385550239607, 6.992620115222774047 ) ) ;
#1399 = CARTESIAN_POINT ( 'NONE',  ( 0.000000000000000000, -4.330127018922193649, -2.500000000000000000 ) ) ;
#1400 = ORIENTED_EDGE ( 'NONE', *, *, #11817, .F. ) ;
#1401 = CIRCLE ( 'NONE', #8276, 8.105212085995399107 ) ;
#1402 = EDGE_LOOP ( 'NONE', ( #7892, #3977 ) ) ;
#1403 = APPLICATION_CONTEXT ( 'automotive_design' ) ;
#1404 = EDGE_CURVE ( 'NONE', #10542, #9688, #11623, .T. ) ;
#1405 = CIRCLE ( 'NONE', #10911, 4.799999999999999822 ) ;
#1406 = VERTEX_POINT ( 'NONE', #9475 ) ;
#1407 = DIRECTION ( 'NONE',  ( 1.000000000000000000, 0.000000000000000000, 0.000000000000000000 ) ) ;
#1408 = AXIS2_PLACEMENT_3D ( 'NONE', #6301, #1005, #7116 ) ;
#1409 = CARTESIAN_POINT ( 'NONE',  ( 1.360585162435110629, -4.061296242128317857, -3.505054077164905024 ) ) ;
#1410 = DIRECTION ( 'NONE',  ( -0.000000000000000000, -0.000000000000000000, -1.000000000000000000 ) ) ;
#1411 = SHAPE_REPRESENTATION_RELATIONSHIP ( 'NONE' , 'NONE' ,  #8584, #2368 ) ;
#1412 = CARTESIAN_POINT ( 'NONE',  ( 6.323279575526388641, 5.335162385629701909, 0.7592276814629709270 ) ) ;
#1413 = CARTESIAN_POINT ( 'NONE',  ( -18.00000000000000355, -19.99999999999999289, -12.00000000000000000 ) ) ;
#1414 = CIRCLE ( 'NONE', #10486, 4.799999999999999822 ) ;
#1415 = CARTESIAN_POINT ( 'NONE',  ( 57.36023556966787851, 51.00051614449763804, 0.02388180880515038476 ) ) ;
#1416 = DIRECTION ( 'NONE',  ( 0.6040472319084893016, -0.7969485188038759604, -1.107688701425240251E-17 ) ) ;
#1417 = CARTESIAN_POINT ( 'NONE',  ( 54.09612160359786515, 51.69948385550240744, -5.676469297603166098 ) ) ;
#1418 = CARTESIAN_POINT ( 'NONE',  ( 45.90387839640214196, 46.69948385550240744, 5.676469297603166098 ) ) ;
#1419 = VECTOR ( 'NONE', #636, 1000.000000000000000 ) ;
#1420 = CARTESIAN_POINT ( 'NONE',  ( 55.94051828345050836, 45.79948385550240886, -4.345558710429104465 ) ) ;
#1421 = VERTEX_POINT ( 'NONE', #12715 ) ;
#1422 = EDGE_LOOP ( 'NONE', ( #5240, #8901, #12422, #11501, #9871, #1222 ) ) ;
#1423 = CARTESIAN_POINT ( 'NONE',  ( 4.033895293471413623, 1.419609371826631827, -3.500000000000000000 ) ) ;
#1424 = ORIENTED_EDGE ( 'NONE', *, *, #9057, .T. ) ;
#1425 = CARTESIAN_POINT ( 'NONE',  ( 6.897297840755645792E-16, -2.686816014504582739, -2.346298152288354366 ) ) ;
#1426 = EDGE_CURVE ( 'NONE', #11691, #3041, #5274, .T. ) ;
#1427 = DIRECTION ( 'NONE',  ( 1.000000000000000000, -0.000000000000000000, 0.000000000000000000 ) ) ;
#1428 = CARTESIAN_POINT ( 'NONE',  ( 56.30877334542961421, 53.00051614449765935, 0.02388180880515774693 ) ) ;
#1429 = CARTESIAN_POINT ( 'NONE',  ( -20.00000000000000000, -19.99999999999999289, -20.00000000000000000 ) ) ;
#1430 = CARTESIAN_POINT ( 'NONE',  ( 57.60143344285433642, 55.89948385550241028, -2.493737253992118319 ) ) ;
#1431 = CARTESIAN_POINT ( 'NONE',  ( 43.34962307344081012, 54.89948385550240317, 2.184720259617164650 ) ) ;
#1432 = FACE_OUTER_BOUND ( 'NONE', #10283, .T. ) ;
#1433 = CARTESIAN_POINT ( 'NONE',  ( 41.58830220609386430, 64.00051614449765225, -0.02388180880514929535 ) ) ;
#1434 = ORIENTED_EDGE ( 'NONE', *, *, #9580, .T. ) ;
#1435 = EDGE_CURVE ( 'NONE', #5823, #6584, #2129, .T. ) ;
#1436 = EDGE_LOOP ( 'NONE', ( #11212, #8239, #723, #12909 ) ) ;
#1437 = CIRCLE ( 'NONE', #7657, 2.500000000000000444 ) ;
#1438 = ADVANCED_FACE ( 'NONE', ( #71 ), #7660, .F. ) ;
#1439 = ORIENTED_EDGE ( 'NONE', *, *, #1549, .F. ) ;
#1440 = ORIENTED_EDGE ( 'NONE', *, *, #7392, .T. ) ;
#1441 = VECTOR ( 'NONE', #2350, 1000.000000000000000 ) ;
#1442 = DIRECTION ( 'NONE',  ( 0.000000000000000000, -1.000000000000000000, -0.000000000000000000 ) ) ;
#1443 = CYLINDRICAL_SURFACE ( 'NONE', #12538, 12.49999999999999645 ) ;
#1444 = SURFACE_SIDE_STYLE ('',( #12107 ) ) ;
#1445 = CARTESIAN_POINT ( 'NONE',  ( -31.74999999999995737, 0.000000000000000000, 0.000000000000000000 ) ) ;
#1446 = FACE_BOUND ( 'NONE', #1985, .T. ) ;
#1447 = CARTESIAN_POINT ( 'NONE',  ( 48.07319477248768180, 58.59948385550239891, 6.007379884777225953 ) ) ;
#1448 = CARTESIAN_POINT ( 'NONE',  ( 54.13287192849671214, 46.70051614449766220, -5.649768623646139964 ) ) ;
#1449 = B_SPLINE_CURVE_WITH_KNOTS ( 'NONE', 3,
 ( #4192, #1252, #3155, #8415, #7382, #12810, #8611, #8480, #12620, #4386, #8546, #7445, #3223, #105, #6416, #6289 ),
 .UNSPECIFIED., .F., .F.,
 ( 4, 3, 3, 3, 3, 4 ),
 ( -2.111273352581767125E-06, 0.000000000000000000, 3.519286887793215919E-05, 7.191842652067064129E-05, 0.0001049868727093590168, 0.0001382836236822123786 ),
 .UNSPECIFIED. ) ;
#1450 = CARTESIAN_POINT ( 'NONE',  ( 42.38452918213190657, 55.90051614449766504, 2.450534656007115508 ) ) ;
#1451 = FACE_OUTER_BOUND ( 'NONE', #12593, .T. ) ;
#1452 = DIRECTION ( 'NONE',  ( 1.000000000000000000, 3.469446951953615175E-16, 0.000000000000000000 ) ) ;
#1453 = AXIS2_PLACEMENT_3D ( 'NONE', #814, #10307, #1086 ) ;
#1454 = CARTESIAN_POINT ( 'NONE',  ( 42.38452918213190657, 45.90051614449766504, 2.450534656007115508 ) ) ;
#1455 = ORIENTED_EDGE ( 'NONE', *, *, #12136, .F. ) ;
#1456 = EDGE_CURVE ( 'NONE', #11270, #13379, #3187, .T. ) ;
#1457 = DIRECTION ( 'NONE',  ( 1.000000000000000000, 0.000000000000000000, 0.000000000000000000 ) ) ;
#1458 = ORIENTED_EDGE ( 'NONE', *, *, #5839, .F. ) ;
#1459 = PRODUCT_DEFINITION_SHAPE ( 'NONE', 'NONE',  #12493 ) ;
#1460 = LINE ( 'NONE', #5706, #13111 ) ;
#1461 = DIRECTION ( 'NONE',  ( 1.000000000000000000, 3.469446951953615668E-16, -0.000000000000000000 ) ) ;
#1462 = DIRECTION ( 'NONE',  ( 1.000000000000000000, 0.000000000000000000, 0.000000000000000000 ) ) ;
#1463 = CARTESIAN_POINT ( 'NONE',  ( 54.09612160359786515, 59.69948385550240033, -5.676469297603166098 ) ) ;
#1464 = EDGE_CURVE ( 'NONE', #11796, #9525, #9423, .T. ) ;
#1465 = CARTESIAN_POINT ( 'NONE',  ( 44.88205777487401349, 59.80051614449766362, 3.688883143319584779 ) ) ;
#1466 = DIRECTION ( 'NONE',  ( -1.000000000000000000, 0.000000000000000000, 0.000000000000000000 ) ) ;
#1467 = PLANE ( 'NONE',  #5074 ) ;
#1468 = CARTESIAN_POINT ( 'NONE',  ( 56.66441430157294690, 46.90051614449765793, -2.141517661632166281 ) ) ;
#1469 = CARTESIAN_POINT ( 'NONE',  ( 50.02271294988511841, 48.49948385550241170, 6.000000000000000888 ) ) ;
#1470 = CARTESIAN_POINT ( 'NONE',  ( -2.000000000000006661, 3.464101615137750834, 0.000000000000000000 ) ) ;
#1471 = ORIENTED_EDGE ( 'NONE', *, *, #7707, .F. ) ;
#1472 = UNCERTAINTY_MEASURE_WITH_UNIT (LENGTH_MEASURE( 1.000000000000000082E-05 ), #7653, 'distance_accuracy_value', 'NONE');
#1473 = ORIENTED_EDGE ( 'NONE', *, *, #11540, .F. ) ;
#1474 = DIRECTION ( 'NONE',  ( -4.082155997157844188E-16, 1.000000000000000000, 0.000000000000000000 ) ) ;
#1475 = CARTESIAN_POINT ( 'NONE',  ( 62.49999999999998579, 45.00000000000001421, 15.00000000000000000 ) ) ;
#1476 = CARTESIAN_POINT ( 'NONE',  ( 54.89903213687075834, 44.74560054925188268, -5.000000000000007105 ) ) ;
#1477 =( NAMED_UNIT ( * ) SI_UNIT ( $, .STERADIAN. ) SOLID_ANGLE_UNIT ( ) );
#1478 = FACE_OUTER_BOUND ( 'NONE', #9905, .T. ) ;
#1479 = CARTESIAN_POINT ( 'NONE',  ( 4.114405500665260895, -2.025575754679711071, 3.508400121684938089 ) ) ;
#1480 = CARTESIAN_POINT ( 'NONE',  ( 52.25172492374527877, 55.40051614449764372, 7.007379884777203749 ) ) ;
#1481 = DIRECTION ( 'NONE',  ( -0.000000000000000000, -0.000000000000000000, -1.000000000000000000 ) ) ;
#1482 = CARTESIAN_POINT ( 'NONE',  ( 57.36023556966787851, 53.99948385550239038, -0.02388180880522424582 ) ) ;
#1483 = CARTESIAN_POINT ( 'NONE',  ( 54.13287192849676188, 48.29948385550240175, 5.649768623646098220 ) ) ;
#1484 = VECTOR ( 'NONE', #9958, 1000.000000000000000 ) ;
#1485 = CARTESIAN_POINT ( 'NONE',  ( 42.38452918213188525, 65.09948385550239891, -2.450534656007040013 ) ) ;
#1486 = ORIENTED_EDGE ( 'NONE', *, *, #1877, .F. ) ;
#1487 = ORIENTED_EDGE ( 'NONE', *, *, #7648, .T. ) ;
#1488 = DIRECTION ( 'NONE',  ( 0.8571673013836855759, 1.049727191973305147E-16, -0.5150380737757258576 ) ) ;
#1489 = VERTEX_POINT ( 'NONE', #2987 ) ;
#1490 = CARTESIAN_POINT ( 'NONE',  ( -4.000000000000000000, -2.309401076758512694, -3.433295621305382461 ) ) ;
#1491 = AXIS2_PLACEMENT_3D ( 'NONE', #7044, #8152, #5045 ) ;
#1492 = FACE_OUTER_BOUND ( 'NONE', #8858, .T. ) ;
#1493 =( BOUNDED_SURFACE ( )  B_SPLINE_SURFACE ( 3, 2, ( 
 ( #12623, #9246, #10548 ),
 ( #4196, #1059, #9315 ),
 ( #5311, #6150, #41 ),
 ( #13438, #4266, #5178 ),
 ( #12486, #8483, #857 ),
 ( #9388, #3021, #12686 ) ),
 .UNSPECIFIED., .F., .F., .F. ) 
 B_SPLINE_SURFACE_WITH_KNOTS ( ( 4, 2, 4 ),
 ( 3, 3 ),
 ( 0.02032853247518125531, 0.02278863295364820865, 0.02524873343211516200 ),
 ( 0.000000000000000000, 1.000000000000000000 ),
 .UNSPECIFIED. ) 
 GEOMETRIC_REPRESENTATION_ITEM ( )  RATIONAL_B_SPLINE_SURFACE ( (
 ( 1.000000000000000000, 0.8047781615896836271, 1.000000000000000000),
 ( 1.000000000000000000, 0.8123767586289967202, 1.000000000000000000),
 ( 1.000000000000000000, 0.8190662415563443322, 1.000000000000000000),
 ( 1.000000000000000000, 0.8192361015669982205, 1.000000000000000000),
 ( 1.000000000000000000, 0.8126135807103181952, 1.000000000000000000),
 ( 1.000000000000000000, 0.8047712338318587788, 1.000000000000000000) ) ) 
 REPRESENTATION_ITEM ( '' )  SURFACE ( )  );
#1494 = VECTOR ( 'NONE', #3161, 1000.000000000000000 ) ;
#1495 = CARTESIAN_POINT ( 'NONE',  ( 53.50833635130544508, 57.30051614449767072, 4.867452303228181343 ) ) ;
#1496 = LINE ( 'NONE', #9945, #8636 ) ;
#1497 = CARTESIAN_POINT ( 'NONE',  ( 57.61547081786812896, 54.09948385550241312, 2.450534656007040901 ) ) ;
#1498 = CARTESIAN_POINT ( 'NONE',  ( 44.05948171654949874, 58.79948385550240886, 4.345558710429105354 ) ) ;
#1499 = LINE ( 'NONE', #13053, #9995 ) ;
#1500 = EDGE_CURVE ( 'NONE', #2486, #10197, #9207, .T. ) ;
#1501 = CARTESIAN_POINT ( 'NONE',  ( 47.37792948025170858, 61.60051614449765367, 7.992620115222797139 ) ) ;
#1502 = VECTOR ( 'NONE', #9309, 1000.000000000000000 ) ;
#1503 = ORIENTED_EDGE ( 'NONE', *, *, #11929, .F. ) ;
#1504 = ITEM_DEFINED_TRANSFORMATION ( 'NONE', 'NONE', #13005,  #430 ) ;
#1505 = AXIS2_PLACEMENT_3D ( 'NONE', #10752, #2313, #13087 ) ;
#1506 = ORIENTED_EDGE ( 'NONE', *, *, #8296, .T. ) ;
#1507 = ORIENTED_EDGE ( 'NONE', *, *, #5001, .T. ) ;
#1508 = VERTEX_POINT ( 'NONE', #6256 ) ;
#1509 = CARTESIAN_POINT ( 'NONE',  ( 6.534838248920897819, 2.951765777552411318, -5.112608298763837489 ) ) ;
#1510 = DIRECTION ( 'NONE',  ( 1.000000000000000000, 0.000000000000000000, 0.000000000000000000 ) ) ;
#1511 = EDGE_CURVE ( 'NONE', #7656, #12408, #1806, .T. ) ;
#1512 = PRESENTATION_STYLE_ASSIGNMENT (( #6791 ) ) ;
#1513 = DIRECTION ( 'NONE',  ( 1.000000000000000000, 0.000000000000000000, 0.000000000000000000 ) ) ;
#1514 = EDGE_CURVE ( 'NONE', #13345, #4029, #4299, .T. ) ;
#1515 = DIRECTION ( 'NONE',  ( -1.000000000000000000, 0.000000000000000000, 0.000000000000000000 ) ) ;
#1516 = AXIS2_PLACEMENT_3D ( 'NONE', #9631, #7302, #11509 ) ;
#1517 = CARTESIAN_POINT ( 'NONE',  ( 55.71335778527780747, 54.09948385550241312, 1.832500667257165983 ) ) ;
#1518 = CARTESIAN_POINT ( 'NONE',  ( 43.33558569842706021, 47.90051614449765793, 2.141517661632167169 ) ) ;
#1519 = EDGE_CURVE ( 'NONE', #9950, #8373, #6946, .T. ) ;
#1520 = CARTESIAN_POINT ( 'NONE',  ( 45.31609314410960820, 54.30051614449765651, -6.485486291978072693 ) ) ;
#1521 = EDGE_CURVE ( 'NONE', #4218, #582, #5409, .T. ) ;
#1522 = CARTESIAN_POINT ( 'NONE',  ( 5.599999999999999645, -4.041451884327386779, 0.000000000000000000 ) ) ;
#1523 = FACE_OUTER_BOUND ( 'NONE', #4743, .T. ) ;
#1524 = CARTESIAN_POINT ( 'NONE',  ( 42.63976443033212860, 62.00051614449764514, -0.02388180880514948964 ) ) ;
#1525 = ORIENTED_EDGE ( 'NONE', *, *, #12483, .F. ) ;
#1526 = AXIS2_PLACEMENT_3D ( 'NONE', #3445, #1481, #13036 ) ;
#1527 = CARTESIAN_POINT ( 'NONE',  ( -1.828356344711647319, -3.563200125723192002, -1.076197711133951296E-14 ) ) ;
#1528 = ORIENTED_EDGE ( 'NONE', *, *, #7291, .F. ) ;
#1529 = ADVANCED_BREP_SHAPE_REPRESENTATION ( '', ( #10251, #430 ), #10167 ) ;
#1530 = CARTESIAN_POINT ( 'NONE',  ( 7.499999999999834799, -7.009618943233325794, -9.000000000000000000 ) ) ;
#1531 = CARTESIAN_POINT ( 'NONE',  ( 3.958484000407238579, -3.734437307742088485, -0.5317648453099828032 ) ) ;
#1532 = DIRECTION ( 'NONE',  ( 0.000000000000000000, 0.000000000000000000, 1.000000000000000000 ) ) ;
#1533 = CARTESIAN_POINT ( 'NONE',  ( 45.86712807150323812, 59.29948385550240175, -5.649768623646098220 ) ) ;
#1534 = MECHANICAL_DESIGN_GEOMETRIC_PRESENTATION_REPRESENTATION (  '', ( #5757 ), #7318 ) ;
#1535 = CARTESIAN_POINT ( 'NONE',  ( 51.92680522751238925, 61.40051614449765793, 6.007379884777208190 ) ) ;
#1536 = DIRECTION ( 'NONE',  ( 0.1305261922200524616, -0.9914448613738103822, 0.000000000000000000 ) ) ;
#1537 = PLANE ( 'NONE',  #6404 ) ;
#1538 = CARTESIAN_POINT ( 'NONE',  ( 55.94051828345053679, 47.20051614449766220, 4.345558710429044069 ) ) ;
#1539 = CARTESIAN_POINT ( 'NONE',  ( 55.96859303347804371, 64.19948385550239323, 4.306917132069425946 ) ) ;
#1540 = FACE_OUTER_BOUND ( 'NONE', #3449, .T. ) ;
#1541 = ORIENTED_EDGE ( 'NONE', *, *, #8366, .F. ) ;
#1542 = VERTEX_POINT ( 'NONE', #8362 ) ;
#1543 = PLANE ( 'NONE',  #1267 ) ;
#1544 = CIRCLE ( 'NONE', #12812, 8.099999999999999645 ) ;
#1545 = CARTESIAN_POINT ( 'NONE',  ( 62.50000000000000000, 32.50000000000001421, -15.00000000000000000 ) ) ;
#1546 = CARTESIAN_POINT ( 'NONE',  ( -3.734041964264191549, -23.01611183630746638, -8.999999999999996447 ) ) ;
#1547 = LINE ( 'NONE', #3645, #6476 ) ;
#1548 = CARTESIAN_POINT ( 'NONE',  ( 12.17636723815371447, -11.24008670809939581, 9.000000000000000000 ) ) ;
#1549 = EDGE_CURVE ( 'NONE', #6599, #6478, #2894, .T. ) ;
#1550 = CARTESIAN_POINT ( 'NONE',  ( 43.33558569842706021, 61.90051614449766504, 2.141517661632167169 ) ) ;
#1551 = CARTESIAN_POINT ( 'NONE',  ( 6.507056081706568129, -2.993351035583803110, -4.999999999999999112 ) ) ;
#1552 = CARTESIAN_POINT ( 'NONE',  ( 62.50000000000000000, 20.00000000000001421, 15.00000000000000000 ) ) ;
#1553 = CARTESIAN_POINT ( 'NONE',  ( 47.74827507625478518, 52.59948385550239180, 7.007379884777227730 ) ) ;
#1554 = CARTESIAN_POINT ( 'NONE',  ( 54.09612160359786515, 45.69948385550240744, -5.676469297603166098 ) ) ;
#1555 = VECTOR ( 'NONE', #6821, 999.9999999999998863 ) ;
#1556 = CARTESIAN_POINT ( 'NONE',  ( 43.20883090819745576, 62.79948385550240175, 4.963592699179006473 ) ) ;
#1557 = ORIENTED_EDGE ( 'NONE', *, *, #3321, .F. ) ;
#1558 = VERTEX_POINT ( 'NONE', #6097 ) ;
#1559 = LINE ( 'NONE', #6977, #4152 ) ;
#1560 = ORIENTED_EDGE ( 'NONE', *, *, #2352, .F. ) ;
#1561 = LINE ( 'NONE', #6772, #1866 ) ;
#1562 = VECTOR ( 'NONE', #12045, 1000.000000000000000 ) ;
#1563 = AXIS2_PLACEMENT_3D ( 'NONE', #6311, #8038, #3749 ) ;
#1564 = VECTOR ( 'NONE', #4461, 1000.000000000000000 ) ;
#1565 = CARTESIAN_POINT ( 'NONE',  ( 5.991014884144049368, -4.330127018922197202, -2.500000000000000444 ) ) ;
#1566 = CARTESIAN_POINT ( 'NONE',  ( 55.71335778527780036, 54.90051614449765793, -1.832500667257213056 ) ) ;
#1567 = CARTESIAN_POINT ( 'NONE',  ( 3.999999999999998224, 2.472263674411418588, -3.687027874309861897 ) ) ;
#1568 = CARTESIAN_POINT ( 'NONE',  ( 43.20883090819745576, 52.79948385550240175, 4.963592699179006473 ) ) ;
#1569 = CARTESIAN_POINT ( 'NONE',  ( 42.63976443033212860, 54.99948385550241170, 0.02388180880522514787 ) ) ;
#1570 = CARTESIAN_POINT ( 'NONE',  ( -4.000000000000000000, 2.309401076758498483, -3.433295621305379353 ) ) ;
#1571 = CARTESIAN_POINT ( 'NONE',  ( 47.42335538002188144, 46.59948385550239891, 8.007379884777233059 ) ) ;
#1572 = CIRCLE ( 'NONE', #5145, 4.000000000000000000 ) ;
#1573 = VECTOR ( 'NONE', #6134, 1000.000000000000000 ) ;
#1574 = EDGE_LOOP ( 'NONE', ( #3279, #705, #2695, #5481, #5837, #7241, #9903, #9024 ) ) ;
#1575 = ITEM_DEFINED_TRANSFORMATION ( 'NONE', 'NONE', #9278,  #430 ) ;
#1576 = EDGE_LOOP ( 'NONE', ( #9237, #13205, #11519, #1067, #3030, #7455, #3687, #13521, #13342, #12302, #6157, #9485, #5285, #1577, #6093, #1560 ) ) ;
#1577 = ORIENTED_EDGE ( 'NONE', *, *, #662, .F. ) ;
#1578 = ORIENTED_EDGE ( 'NONE', *, *, #11357, .T. ) ;
#1579 = CARTESIAN_POINT ( 'NONE',  ( 32.49999999999998579, 45.00000000000001421, -4.999999999999996447 ) ) ;
#1580 = B_SPLINE_CURVE_WITH_KNOTS ( 'NONE', 3,
 ( #7396, #3438, #2322, #1213, #2386, #4405, #54, #8627 ),
 .UNSPECIFIED., .F., .F.,
 ( 4, 2, 2, 4 ),
 ( 7.780516681398759253E-20, 0.002450665683189819696, 0.003675998524784729327, 0.004901331366379639391 ),
 .UNSPECIFIED. ) ;
#1581 = CARTESIAN_POINT ( 'NONE',  ( 4.052424581287787042, 2.393186648133419414, -2.990837702970412959 ) ) ;
#1582 = DIRECTION ( 'NONE',  ( -0.8660254037844412611, 0.4999999999999956146, 0.000000000000000000 ) ) ;
#1583 = CARTESIAN_POINT ( 'NONE',  ( -74.99999999999997158, 20.00000000000001421, -15.00000000000000000 ) ) ;
#1584 = CARTESIAN_POINT ( 'NONE',  ( 43.69122665457040000, 58.99948385550239749, 0.02388180880521036456 ) ) ;
#1585 = CARTESIAN_POINT ( 'NONE',  ( 56.66441430157294690, 48.90051614449766504, -2.141517661632166281 ) ) ;
#1586 = CARTESIAN_POINT ( 'NONE',  ( 45.27934281921082516, 53.70051614449766220, 6.458785618021089192 ) ) ;
#1587 = AXIS2_PLACEMENT_3D ( 'NONE', #2411, #5477, #10718 ) ;
#1588 =( LENGTH_UNIT ( ) NAMED_UNIT ( * ) SI_UNIT ( .MILLI., .METRE. ) );
#1589 = DIRECTION ( 'NONE',  ( 0.000000000000000000, 0.000000000000000000, -1.000000000000000000 ) ) ;
#1590 = CARTESIAN_POINT ( 'NONE',  ( 55.96859303347802239, 60.80051614449764941, -4.306917132069484566 ) ) ;
#1591 = CIRCLE ( 'NONE', #10443, 2.649999999999985700 ) ;
#1592 = ORIENTED_EDGE ( 'NONE', *, *, #4472, .T. ) ;
#1593 = CARTESIAN_POINT ( 'NONE',  ( 1.734723475976807094E-15, 4.618802153517012954, -0.4999999999999995559 ) ) ;
#1594 = B_SPLINE_CURVE_WITH_KNOTS ( 'NONE', 3,
 ( #2150, #8591, #8332, #6270, #6334, #8395 ),
 .UNSPECIFIED., .F., .F.,
 ( 4, 2, 4 ),
 ( 0.01506847346324404271, 0.01653041426658209689, 0.01799235506992015107 ),
 .UNSPECIFIED. ) ;
#1595 = ORIENTED_EDGE ( 'NONE', *, *, #6697, .T. ) ;
#1596 = AXIS2_PLACEMENT_3D ( 'NONE', #10297, #1999, #9268 ) ;
#1597 = DIRECTION ( 'NONE',  ( 1.000000000000000000, -0.000000000000000000, -0.000000000000000000 ) ) ;
#1598 = CARTESIAN_POINT ( 'NONE',  ( 6.207682235857189035, 2.016324304256315258, 4.999999999999999112 ) ) ;
#1599 = CARTESIAN_POINT ( 'NONE',  ( 45.86712807150323812, 57.29948385550240175, -5.649768623646098220 ) ) ;
#1600 = CARTESIAN_POINT ( 'NONE',  ( 54.13287192849676188, 52.29948385550240886, 5.649768623646098220 ) ) ;
#1601 = CARTESIAN_POINT ( 'NONE',  ( 44.88205777487401349, 57.80051614449766362, 3.688883143319584779 ) ) ;
#1602 = LINE ( 'NONE', #12470, #5242 ) ;
#1603 = FACE_OUTER_BOUND ( 'NONE', #7658, .T. ) ;
#1604 = CARTESIAN_POINT ( 'NONE',  ( 51.92680522751238925, 63.40051614449765083, 6.007379884777208190 ) ) ;
#1605 = CARTESIAN_POINT ( 'NONE',  ( 51.97223112728254790, 46.39948385550240317, 5.992620115222778487 ) ) ;
#1606 = DIRECTION ( 'NONE',  ( 1.000000000000000000, 0.000000000000000000, 0.000000000000000000 ) ) ;
#1607 = ORIENTED_EDGE ( 'NONE', *, *, #769, .T. ) ;
#1608 = UNCERTAINTY_MEASURE_WITH_UNIT (LENGTH_MEASURE( 1.000000000000000082E-05 ), #10444, 'distance_accuracy_value', 'NONE');
#1609 = EDGE_LOOP ( 'NONE', ( #9856, #13113, #12373, #3824, #12071, #9555 ) ) ;
#1611 = EDGE_CURVE ( 'NONE', #13245, #504, #728, .T. ) ;
#1610 = ORIENTED_EDGE ( 'NONE', *, *, #10696, .T. ) ;
#1612 = CARTESIAN_POINT ( 'NONE',  ( 8.500000000000000000, 0.000000000000000000, 0.000000000000000000 ) ) ;
#1613 = EDGE_CURVE ( 'NONE', #10197, #2486, #13552, .T. ) ;
#1614 = DIRECTION ( 'NONE',  ( -0.000000000000000000, -0.000000000000000000, 1.000000000000000000 ) ) ;
#1615 = DIRECTION ( 'NONE',  ( 0.3420201433256622736, 1.150791560227853228E-16, 0.9396926207859106484 ) ) ;
#1616 = SURFACE_STYLE_FILL_AREA ( #7027 ) ;
#1617 = DIRECTION ( 'NONE',  ( 0.000000000000000000, 0.000000000000000000, -1.000000000000000000 ) ) ;
#1618 = ADVANCED_FACE ( 'NONE', ( #3928 ), #9260, .F. ) ;
#1619 = DIRECTION ( 'NONE',  ( -0.000000000000000000, -0.000000000000000000, 1.000000000000000000 ) ) ;
#1620 = AXIS2_PLACEMENT_3D ( 'NONE', #4593, #5570, #8747 ) ;
#1621 = CARTESIAN_POINT ( 'NONE',  ( 56.65037692655921120, 61.10051614449766078, 2.184720259617097593 ) ) ;
#1622 = CARTESIAN_POINT ( 'NONE',  ( -1.000000000000000000, -14.00000000000000000, 8.999999999999998224 ) ) ;
#1623 = CARTESIAN_POINT ( 'NONE',  ( 3.951447005078450925, 3.704664227300100254, -0.5833333333333329263 ) ) ;
#1624 = AXIS2_PLACEMENT_3D ( 'NONE', #5236, #4184, #12612 ) ;
#1625 = CARTESIAN_POINT ( 'NONE',  ( 54.09612160359786515, 59.69948385550240033, -5.676469297603166098 ) ) ;
#1626 = CARTESIAN_POINT ( 'NONE',  ( 44.03140696652192787, 49.19948385550240033, -4.306917132069425058 ) ) ;
#1627 = CARTESIAN_POINT ( 'NONE',  ( 52.25172492374522903, 51.59948385550240602, -7.007379884777225953 ) ) ;
#1628 = AXIS2_PLACEMENT_3D ( 'NONE', #13208, #1322, #6741 ) ;
#1629 = ORIENTED_EDGE ( 'NONE', *, *, #284, .F. ) ;
#1630 = ORIENTED_EDGE ( 'NONE', *, *, #5441, .F. ) ;
#1631 = CARTESIAN_POINT ( 'NONE',  ( 20.00000000000000000, -20.00000000000000000, -20.00000000000000000 ) ) ;
#1632 = ORIENTED_EDGE ( 'NONE', *, *, #12015, .T. ) ;
#1633 = CARTESIAN_POINT ( 'NONE',  ( -74.99999999999997158, -7.499999999999971578, -20.00000000000000000 ) ) ;
#1634 = VECTOR ( 'NONE', #8286, 1000.000000000000000 ) ;
#1635 = LINE ( 'NONE', #584, #5083 ) ;
#1636 = CARTESIAN_POINT ( 'NONE',  ( 44.91013252490150620, 60.20051614449766220, -3.727524721679154940 ) ) ;
#1637 = DIRECTION ( 'NONE',  ( -1.000000000000000000, 0.000000000000000000, 0.000000000000000000 ) ) ;
#1638 = CIRCLE ( 'NONE', #6092, 15.00000000000000000 ) ;
#1639 = CARTESIAN_POINT ( 'NONE',  ( 52.62207051974839089, 58.39948385550241028, 7.992620115222770494 ) ) ;
#1640 = ADVANCED_FACE ( 'NONE', ( #5191 ), #6734, .T. ) ;
#1641 = CARTESIAN_POINT ( 'NONE',  ( 43.34962307344081012, 60.89948385550241028, 2.184720259617164650 ) ) ;
#1642 = FACE_BOUND ( 'NONE', #9538, .T. ) ;
#1643 = CARTESIAN_POINT ( 'NONE',  ( 56.79116909180259398, 63.20051614449766220, 4.963592699178938972 ) ) ;
#1644 = ORIENTED_EDGE ( 'NONE', *, *, #4617, .F. ) ;
#1645 = ORIENTED_EDGE ( 'NONE', *, *, #7550, .F. ) ;
#1646 = ORIENTED_EDGE ( 'NONE', *, *, #12351, .F. ) ;
#1647 = ORIENTED_EDGE ( 'NONE', *, *, #668, .T. ) ;
#1648 = DIRECTION ( 'NONE',  ( 0.8660254037844381525, 0.5000000000000009992, 0.000000000000000000 ) ) ;
#1649 = EDGE_CURVE ( 'NONE', #12919, #5687, #13118, .T. ) ;
#1650 = EDGE_CURVE ( 'NONE', #4030, #12154, #7403, .T. ) ;
#1651 = CARTESIAN_POINT ( 'NONE',  ( -59.84999999999998721, 32.50000000000001421, -9.999999999999998224 ) ) ;
#1652 = CARTESIAN_POINT ( 'NONE',  ( 4.086376042167605860, 1.979461949354204719, -3.571471332069177773 ) ) ;
#1653 = CARTESIAN_POINT ( 'NONE',  ( 3.333333333333335702, -2.694301256218268215, -3.300726591567084256 ) ) ;
#1654 = CARTESIAN_POINT ( 'NONE',  ( 62.50000000000000000, 32.50000000000001421, 9.999999999999998224 ) ) ;
#1655 = CARTESIAN_POINT ( 'NONE',  ( 46.49166364869460466, 62.69948385550240744, 4.867452303228209765 ) ) ;
#1656 = CARTESIAN_POINT ( 'NONE',  ( 57.36023556966787851, 53.00051614449765225, 0.02388180880515038476 ) ) ;
#1657 = CARTESIAN_POINT ( 'NONE',  ( 42.38452918213190657, 53.90051614449765793, 2.450534656007115508 ) ) ;
#1658 = CARTESIAN_POINT ( 'NONE',  ( 5.560781378645573980, 6.809993116116507654E-16, -4.000000000000000000 ) ) ;
#1659 = DIRECTION ( 'NONE',  ( 0.000000000000000000, 0.000000000000000000, -1.000000000000000000 ) ) ;
#1660 = CARTESIAN_POINT ( 'NONE',  ( 43.34962307344078880, 64.10051614449766078, -2.184720259617096705 ) ) ;
#1661 = PRODUCT_RELATED_PRODUCT_CATEGORY ( 'part', '', ( #13478 ) ) ;
#1663 = ORIENTED_EDGE ( 'NONE', *, *, #10213, .T. ) ;
#1662 = ORIENTED_EDGE ( 'NONE', *, *, #5497, .T. ) ;
#1664 =( BOUNDED_SURFACE ( )  B_SPLINE_SURFACE ( 3, 2, ( 
 ( #13580, #3086, #7317 ),
 ( #992, #5244, #9444 ),
 ( #2105, #6352, #11848 ),
 ( #13081, #10945, #5641 ),
 ( #1598, #9713, #8811 ),
 ( #5707, #8682, #10807 ) ),
 .UNSPECIFIED., .F., .F., .T. ) 
 B_SPLINE_SURFACE_WITH_KNOTS ( ( 4, 2, 4 ),
 ( 3, 3 ),
 ( 0.02367497856332483747, 0.02662799652435013376, 0.02958101448537543005 ),
 ( 0.000000000000000000, 1.000000000000000000 ),
 .UNSPECIFIED. ) 
 GEOMETRIC_REPRESENTATION_ITEM ( )  RATIONAL_B_SPLINE_SURFACE ( (
 ( 1.000000000000000000, 0.8047781226141854649, 1.000000000000000000),
 ( 1.000000000000000000, 0.8123782257049820821, 1.000000000000000000),
 ( 1.000000000000000000, 0.8190665358012705344, 1.000000000000000000),
 ( 1.000000000000000000, 0.8192358187342196896, 1.000000000000000000),
 ( 1.000000000000000000, 0.8126132506074239537, 1.000000000000000000),
 ( 1.000000000000000000, 0.8047712440299316095, 1.000000000000000000) ) ) 
 REPRESENTATION_ITEM ( '' )  SURFACE ( )  );
#1665 = DIRECTION ( 'NONE',  ( 0.8660254037844381525, 0.5000000000000009992, 0.000000000000000000 ) ) ;
#1666 = ORIENTED_EDGE ( 'NONE', *, *, #12441, .F. ) ;
#1667 = DIRECTION ( 'NONE',  ( -0.5000000000000041078, 0.8660254037844362651, 0.000000000000000000 ) ) ;
#1668 = CARTESIAN_POINT ( 'NONE',  ( -9.999999999999994671, 20.00000000000001421, 15.00000000000000000 ) ) ;
#1669 = CIRCLE ( 'NONE', #5891, 4.799999999999999822 ) ;
#1670 = CARTESIAN_POINT ( 'NONE',  ( 55.94051828345050836, 59.79948385550238754, -4.345558710429104465 ) ) ;
#1671 = CARTESIAN_POINT ( 'NONE',  ( 43.34962307344081012, 58.89948385550241028, 2.184720259617164650 ) ) ;
#1672 = VECTOR ( 'NONE', #7417, 1000.000000000000000 ) ;
#1673 = FACE_OUTER_BOUND ( 'NONE', #12257, .T. ) ;
#1674 = FACE_OUTER_BOUND ( 'NONE', #521, .T. ) ;
#1675 = CARTESIAN_POINT ( 'NONE',  ( 0.1481481481481481122, -4.797713218419819903, 0.000000000000000000 ) ) ;
#1676 = CARTESIAN_POINT ( 'NONE',  ( 54.13287192849671214, 46.70051614449766220, -5.649768623646139964 ) ) ;
#1677 = CARTESIAN_POINT ( 'NONE',  ( 55.08986747509847248, 53.79948385550241596, -3.727524721679197572 ) ) ;
#1678 = CARTESIAN_POINT ( 'NONE',  ( 20.00000000000000000, -25.00000000000000711, -23.00000000000000000 ) ) ;
#1679 = ADVANCED_FACE ( 'NONE', ( #871 ), #8157, .F. ) ;
#1680 = ORIENTED_EDGE ( 'NONE', *, *, #8779, .F. ) ;
#1681 = ORIENTED_EDGE ( 'NONE', *, *, #5603, .T. ) ;
#1682 = ORIENTED_EDGE ( 'NONE', *, *, #3729, .F. ) ;
#1683 = FACE_OUTER_BOUND ( 'NONE', #4420, .T. ) ;
#1684 = DIRECTION ( 'NONE',  ( 0.000000000000000000, 0.000000000000000000, 1.000000000000000000 ) ) ;
#1685 = CARTESIAN_POINT ( 'NONE',  ( 6.245824673232814206, -3.903127342723638371, -3.450227696316022996 ) ) ;
#1686 = FILL_AREA_STYLE ('',( #6759 ) ) ;
#1687 = CARTESIAN_POINT ( 'NONE',  ( 6.092449800118089343, 4.833012432206481357, 1.628976913806340798 ) ) ;
#1688 = DIRECTION ( 'NONE',  ( 0.000000000000000000, 0.000000000000000000, 1.000000000000000000 ) ) ;
#1689 = EDGE_CURVE ( 'NONE', #2696, #1895, #4289, .T. ) ;
#1690 = CARTESIAN_POINT ( 'NONE',  ( 52.25172492374527877, 57.40051614449765083, 7.007379884777203749 ) ) ;
#1691 = DIRECTION ( 'NONE',  ( 0.1305261922200524338, 0.9914448613738102711, 0.000000000000000000 ) ) ;
#1692 = CARTESIAN_POINT ( 'NONE',  ( 53.50833635130540955, 63.69948385550240033, -4.867452303228209765 ) ) ;
#1693 = EDGE_CURVE ( 'NONE', #4523, #12971, #6022, .T. ) ;
#1694 = DIRECTION ( 'NONE',  ( -1.000000000000000000, -0.000000000000000000, 0.000000000000000000 ) ) ;
#1695 = CARTESIAN_POINT ( 'NONE',  ( 43.33558569842703179, 59.09948385550240602, -2.141517661632099223 ) ) ;
#1696 = CARTESIAN_POINT ( 'NONE',  ( 47.70284917648453415, 47.39948385550238896, -6.992620115222774047 ) ) ;
#1697 = EDGE_CURVE ( 'NONE', #5890, #11555, #12498, .T. ) ;
#1698 = CARTESIAN_POINT ( 'NONE',  ( 43.33558569842703179, 47.09948385550240602, -2.141517661632099223 ) ) ;
#1699 = ORIENTED_EDGE ( 'NONE', *, *, #4647, .T. ) ;
#1700 = ORIENTED_EDGE ( 'NONE', *, *, #6637, .T. ) ;
#1701 = CARTESIAN_POINT ( 'NONE',  ( 75.00000000000002842, -39.99999999999998579, -10.00000000000000000 ) ) ;
#1702 = EDGE_CURVE ( 'NONE', #13026, #10076, #2059, .T. ) ;
#1703 = ORIENTED_EDGE ( 'NONE', *, *, #10554, .T. ) ;
#1704 = CARTESIAN_POINT ( 'NONE',  ( 17.85000000000000142, -20.00000000000000000, -23.00000000000000000 ) ) ;
#1705 = CARTESIAN_POINT ( 'NONE',  ( 3.972709601346591235, 2.746729940827189242, -2.374099244652734697 ) ) ;
#1706 = CARTESIAN_POINT ( 'NONE',  ( 44.91013252490150620, 64.20051614449766930, -3.727524721679154940 ) ) ;
#1707 = CARTESIAN_POINT ( 'NONE',  ( -75.00000000000001421, 4.999999999999974243, 0.000000000000000000 ) ) ;
#1708 = EDGE_CURVE ( 'NONE', #9272, #8675, #5122, .T. ) ;
#1709 = CARTESIAN_POINT ( 'NONE',  ( 45.31609314410967926, 56.69948385550240744, 6.485486291978119766 ) ) ;
#1710 = ADVANCED_FACE ( 'NONE', ( #1919 ), #4982, .T. ) ;
#1711 = DIRECTION ( 'NONE',  ( 0.000000000000000000, 0.000000000000000000, 1.000000000000000000 ) ) ;
#1712 = FACE_OUTER_BOUND ( 'NONE', #12953, .T. ) ;
#1713 = CARTESIAN_POINT ( 'NONE',  ( 45.27934281921075410, 49.29948385550240886, -6.458785618021043895 ) ) ;
#1714 = ORIENTED_EDGE ( 'NONE', *, *, #9304, .F. ) ;
#1715 = ORIENTED_EDGE ( 'NONE', *, *, #3585, .F. ) ;
#1716 = EDGE_LOOP ( 'NONE', ( #232, #7425, #4993, #9885, #7605, #12254, #2606, #5059 ) ) ;
#1717 = VECTOR ( 'NONE', #3029, 1000.000000000000000 ) ;
#1718 = ORIENTED_EDGE ( 'NONE', *, *, #1708, .F. ) ;
#1719 = DIRECTION ( 'NONE',  ( -1.000000000000000000, 0.000000000000000000, 0.000000000000000000 ) ) ;
#1720 = LINE ( 'NONE', #9068, #8575 ) ;
#1721 = SURFACE_STYLE_USAGE ( .BOTH. , #9137 ) ;
#1722 = CARTESIAN_POINT ( 'NONE',  ( 5.599999999999999645, -2.020725942163686284, 3.500000000000000444 ) ) ;
#1723 = DIRECTION ( 'NONE',  ( 0.000000000000000000, 0.8660254037844380415, -0.5000000000000012212 ) ) ;
#1724 = CARTESIAN_POINT ( 'NONE',  ( -2.649999999999988365, 15.00000000000001599, 9.000000000000000000 ) ) ;
#1725 = CARTESIAN_POINT ( 'NONE',  ( 48.02776887271745210, 65.39948385550239607, -5.992620115222778487 ) ) ;
#1726 = CARTESIAN_POINT ( 'NONE',  ( 52.29715082351539479, 52.60051614449766078, -6.992620115222796251 ) ) ;
#1727 = CARTESIAN_POINT ( 'NONE',  ( 45.31609314410960820, 56.30051614449766362, -6.485486291978072693 ) ) ;
#1728 = ADVANCED_FACE ( 'NONE', ( #12363 ), #6303, .T. ) ;
#1729 = EDGE_CURVE ( 'NONE', #11948, #11251, #12889, .T. ) ;
#1730 = DIRECTION ( 'NONE',  ( -0.2439756946365075896, 0.9697813467099857254, 1.610118993450814692E-22 ) ) ;
#1731 = CARTESIAN_POINT ( 'NONE',  ( 0.000000000000000000, 0.000000000000000000, 0.000000000000000000 ) ) ;
#1732 = CARTESIAN_POINT ( 'NONE',  ( 42.39856655714564226, 48.10051614449766078, -2.493737253992044156 ) ) ;
#1733 = AXIS2_PLACEMENT_3D ( 'NONE', #7089, #9091, #7918 ) ;
#1735 = VERTEX_POINT ( 'NONE', #7119 ) ;
#1734 = ORIENTED_EDGE ( 'NONE', *, *, #5860, .F. ) ;
#1736 = CARTESIAN_POINT ( 'NONE',  ( 2.000000000000000000, 1.773042676681340524, -2.059984127722458425E-15 ) ) ;
#1737 = ORIENTED_EDGE ( 'NONE', *, *, #5970, .T. ) ;
#1738 = EDGE_LOOP ( 'NONE', ( #9969, #12992 ) ) ;
#1739 = DIRECTION ( 'NONE',  ( -1.000000000000000000, -0.000000000000000000, -0.000000000000000000 ) ) ;
#1740 = DIRECTION ( 'NONE',  ( 1.040834085586083310E-14, -1.000000000000000000, 0.000000000000000000 ) ) ;
#1741 = SHAPE_DEFINITION_REPRESENTATION ( #12618, #11036 ) ;
#1742 = CARTESIAN_POINT ( 'NONE',  ( 51.92680522751233951, 45.59948385550240602, -6.007379884777223289 ) ) ;
#1743 = CARTESIAN_POINT ( 'NONE',  ( 44.03140696652193498, 59.19948385550240033, -4.306917132069424170 ) ) ;
#1744 = CARTESIAN_POINT ( 'NONE',  ( -1.372193374551966155E-15, -2.859595677584338969, 2.047034997319577609 ) ) ;
#1745 = CARTESIAN_POINT ( 'NONE',  ( 2.482347295856823136E-15, -20.00000000000000000, -8.999999999999996447 ) ) ;
#1746 = PRODUCT_DEFINITION_FORMATION_WITH_SPECIFIED_SOURCE ( 'ANY', '', #4005, .NOT_KNOWN. ) ;
#1747 = CARTESIAN_POINT ( 'NONE',  ( 50.00000000000000000, 15.00000000000000000, 0.000000000000000000 ) ) ;
#1748 = CARTESIAN_POINT ( 'NONE',  ( 54.13287192849671214, 44.70051614449766220, -5.649768623646139964 ) ) ;
#1749 = CARTESIAN_POINT ( 'NONE',  ( 46.49166364869460466, 50.69948385550240744, 4.867452303228209765 ) ) ;
#1750 = AXIS2_PLACEMENT_3D ( 'NONE', #3863, #13247, #7885 ) ;
#1751 = DIRECTION ( 'NONE',  ( 1.000000000000000000, 0.000000000000000000, 0.000000000000000000 ) ) ;
#1752 = EDGE_LOOP ( 'NONE', ( #12756, #3736 ) ) ;
#1753 = EDGE_CURVE ( 'NONE', #3958, #5739, #10479, .T. ) ;
#1754 = VERTEX_POINT ( 'NONE', #1274 ) ;
#1755 = ORIENTED_EDGE ( 'NONE', *, *, #13336, .F. ) ;
#1756 = CARTESIAN_POINT ( 'NONE',  ( 13.99999999999999822, 0.000000000000000000, 0.000000000000000000 ) ) ;
#1757 = LINE ( 'NONE', #11528, #5840 ) ;
#1758 = DIRECTION ( 'NONE',  ( -9.858538378746663627E-23, 5.031452844637890958E-23, -1.000000000000000000 ) ) ;
#1759 = PRESENTATION_LAYER_ASSIGNMENT (  '', '', ( #5757 ) ) ;
#1760 = B_SPLINE_CURVE_WITH_KNOTS ( 'NONE', 3,
 ( #5999, #12480, #924, #13578, #8348 ),
 .UNSPECIFIED., .F., .F.,
 ( 4, 1, 4 ),
 ( 0.000000000000000000, 0.002309401076758505356, 0.004618802153517010713 ),
 .UNSPECIFIED. ) ;
#1761 = CARTESIAN_POINT ( 'NONE',  ( 56.66441430157296821, 46.09948385550240602, 2.141517661632100111 ) ) ;
#1762 = CARTESIAN_POINT ( 'NONE',  ( 62.49999999999998579, 45.00000000000001421, -5.000000000000000000 ) ) ;
#1763 = CARTESIAN_POINT ( 'NONE',  ( 6.541171952014627422, 2.986180817377861896, -5.112746308113085725 ) ) ;
#1764 = CARTESIAN_POINT ( 'NONE',  ( 55.11794222512601493, 64.19948385550240744, 3.688883143319541702 ) ) ;
#1765 = CARTESIAN_POINT ( 'NONE',  ( 2.000000000000000000, -1.773042676681341856, 2.276824562219559311E-15 ) ) ;
#1766 = CARTESIAN_POINT ( 'NONE',  ( 52.25172492374522903, 59.59948385550240602, -7.007379884777225953 ) ) ;
#1767 = CARTESIAN_POINT ( 'NONE',  ( 45.86712807150323812, 55.29948385550240175, -5.649768623646098220 ) ) ;
#1768 = ORIENTED_EDGE ( 'NONE', *, *, #9656, .F. ) ;
#1769 = CARTESIAN_POINT ( 'NONE',  ( 57.36023556966787851, 49.99948385550238328, -0.02388180880522424582 ) ) ;
#1770 = CIRCLE ( 'NONE', #5116, 4.000000000000000000 ) ;
#1771 = ORIENTED_EDGE ( 'NONE', *, *, #4489, .F. ) ;
#1772 = ORIENTED_EDGE ( 'NONE', *, *, #9738, .F. ) ;
#1773 = CARTESIAN_POINT ( 'NONE',  ( 3.878089031707363521, 0.7015470581914173831, 3.500000000000000444 ) ) ;
#1774 = EDGE_LOOP ( 'NONE', ( #5944, #2961, #9843, #12955 ) ) ;
#1775 = EDGE_CURVE ( 'NONE', #11894, #614, #6502, .T. ) ;
#1776 = CARTESIAN_POINT ( 'NONE',  ( 4.104070371397480876, 2.023683613428366002, 3.505122836902507810 ) ) ;
#1777 = EDGE_CURVE ( 'NONE', #6619, #9080, #12238, .T. ) ;
#1778 = CARTESIAN_POINT ( 'NONE',  ( 20.00000000000000000, -20.00000000000000000, -20.00000000000000000 ) ) ;
#1779 = DIRECTION ( 'NONE',  ( 0.000000000000000000, 0.000000000000000000, -1.000000000000000000 ) ) ;
#1780 = VECTOR ( 'NONE', #9908, 1000.000000000000000 ) ;
#1781 = CARTESIAN_POINT ( 'NONE',  ( 56.30877334542961421, 61.00051614449765935, 0.02388180880515774693 ) ) ;
#1782 = FACE_OUTER_BOUND ( 'NONE', #10657, .T. ) ;
#1783 = CARTESIAN_POINT ( 'NONE',  ( 43.20883090819745576, 58.79948385550240175, 4.963592699179006473 ) ) ;
#1784 = CARTESIAN_POINT ( 'NONE',  ( 44.05948171654949874, 60.79948385550240886, 4.345558710429105354 ) ) ;
#1785 = DIRECTION ( 'NONE',  ( 0.03086419753086420623, 0.9995235871707959241, 0.000000000000000000 ) ) ;
#1786 = CARTESIAN_POINT ( 'NONE',  ( 50.02271294988513972, 48.49948385550241170, 8.000000000000001776 ) ) ;
#1787 = VERTEX_POINT ( 'NONE', #3373 ) ;
#1788 = ORIENTED_EDGE ( 'NONE', *, *, #132, .T. ) ;
#1789 = ORIENTED_EDGE ( 'NONE', *, *, #8633, .F. ) ;
#1790 = AXIS2_PLACEMENT_3D ( 'NONE', #10437, #10100, #13603 ) ;
#1791 = DIRECTION ( 'NONE',  ( 1.000000000000000000, 0.000000000000000000, -0.000000000000000000 ) ) ;
#1792 = CYLINDRICAL_SURFACE ( 'NONE', #7254, 15.00000000000000000 ) ;
#1793 = ADVANCED_FACE ( 'NONE', ( #252, #186 ), #7462, .F. ) ;
#1794 = LINE ( 'NONE', #2985, #6464 ) ;
#1795 = CARTESIAN_POINT ( 'NONE',  ( 49.99999999999997158, 45.00000000000003553, -7.000000000000000888 ) ) ;
#1796 = CARTESIAN_POINT ( 'NONE',  ( 0.4465819873851989974, -2.886751345948120218, 4.999999999999999112 ) ) ;
#1797 = CARTESIAN_POINT ( 'NONE',  ( 50.02271294988511841, 62.49948385550240459, 6.000000000000000888 ) ) ;
#1798 = EDGE_CURVE ( 'NONE', #10006, #10542, #11868, .T. ) ;
#1799 = CARTESIAN_POINT ( 'NONE',  ( 43.34962307344078880, 56.10051614449766078, -2.184720259617096705 ) ) ;
#1800 = CARTESIAN_POINT ( 'NONE',  ( 45.27934281921082516, 59.70051614449766220, 6.458785618021089192 ) ) ;
#1801 = CIRCLE ( 'NONE', #3579, 7.500000000000000888 ) ;
#1802 = AXIS2_PLACEMENT_3D ( 'NONE', #8195, #12264, #11369 ) ;
#1803 = DIRECTION ( 'NONE',  ( -1.000000000000000000, 0.000000000000000000, 0.000000000000000000 ) ) ;
#1804 = AXIS2_PLACEMENT_3D ( 'NONE', #9785, #7582, #1329 ) ;
#1805 = CARTESIAN_POINT ( 'NONE',  ( 43.18075615816994173, 49.80051614449765651, 4.924951120819380357 ) ) ;
#1806 = B_SPLINE_CURVE_WITH_KNOTS ( 'NONE', 3,
 ( #4155, #10447, #9415, #955 ),
 .UNSPECIFIED., .F., .F.,
 ( 4, 4 ),
 ( 0.002977824986803859555, 0.005972417098209359745 ),
 .UNSPECIFIED. ) ;
#1808 = EDGE_LOOP ( 'NONE', ( #1646, #10556, #3839, #4401 ) ) ;
#1807 = ORIENTED_EDGE ( 'NONE', *, *, #4185, .F. ) ;
#1809 = FACE_OUTER_BOUND ( 'NONE', #13519, .T. ) ;
#1810 = ORIENTED_EDGE ( 'NONE', *, *, #10510, .F. ) ;
#1811 = ORIENTED_EDGE ( 'NONE', *, *, #7648, .F. ) ;
#1812 = VECTOR ( 'NONE', #9209, 1000.000000000000000 ) ;
#1813 = CARTESIAN_POINT ( 'NONE',  ( -14.92499999999998828, -21.49812382665791688, 9.000000000000000000 ) ) ;
#1814 = AXIS2_PLACEMENT_3D ( 'NONE', #4160, #3121, #3952 ) ;
#1815 = SHAPE_DEFINITION_REPRESENTATION ( #1901, #5328 ) ;
#1816 = CARTESIAN_POINT ( 'NONE',  ( 47.70284917648453415, 65.39948385550239607, -6.992620115222774047 ) ) ;
#1817 = CARTESIAN_POINT ( 'NONE',  ( 50.02271294988512551, 56.49948385550240459, 7.000000000000000888 ) ) ;
#1818 = CARTESIAN_POINT ( 'NONE',  ( 75.00000000000001421, -7.499999999999975131, 10.00000000000000000 ) ) ;
#1819 = LINE ( 'NONE', #10329, #2792 ) ;
#1820 = CARTESIAN_POINT ( 'NONE',  ( 52.80949999999998568, 0.000000000000000000, 0.000000000000000000 ) ) ;
#1821 = CARTESIAN_POINT ( 'NONE',  ( 54.09612160359792199, 53.30051614449766362, 5.676469297603124353 ) ) ;
#1822 = CARTESIAN_POINT ( 'NONE',  ( 53.54508667620428497, 54.29948385550241596, 4.840751629271157874 ) ) ;
#1823 = CARTESIAN_POINT ( 'NONE',  ( 0.000000000000000000, 0.000000000000000000, -5.000000000000000000 ) ) ;
#1824 = VERTEX_POINT ( 'NONE', #4409 ) ;
#1825 = AXIS2_PLACEMENT_3D ( 'NONE', #8022, #3667, #7954 ) ;
#1826 = EDGE_LOOP ( 'NONE', ( #11523, #11071, #5516, #8412 ) ) ;
#1827 = EDGE_LOOP ( 'NONE', ( #3789, #7685, #4973, #11985 ) ) ;
#1828 = DIRECTION ( 'NONE',  ( 0.000000000000000000, 0.000000000000000000, 1.000000000000000000 ) ) ;
#1829 = CARTESIAN_POINT ( 'NONE',  ( 6.390983399715591595, 2.822795037344616897, -5.110775575965828210 ) ) ;
#1830 = CARTESIAN_POINT ( 'NONE',  ( -74.99999999999997158, 32.50000000000001421, 15.00000000000000000 ) ) ;
#1831 = AXIS2_PLACEMENT_3D ( 'NONE', #5105, #11240, #6149 ) ;
#1832 = CARTESIAN_POINT ( 'NONE',  ( 45.90387839640214196, 46.69948385550240744, 5.676469297603166098 ) ) ;
#1833 = SURFACE_SIDE_STYLE ('',( #11311 ) ) ;
#1834 = CARTESIAN_POINT ( 'NONE',  ( 6.095462721915160920, 1.047438013718291705, -5.000000000000000000 ) ) ;
#1835 = CARTESIAN_POINT ( 'NONE',  ( 48.07319477248768180, 64.59948385550241312, 6.007379884777225953 ) ) ;
#1836 = DIRECTION ( 'NONE',  ( -0.000000000000000000, -0.000000000000000000, -1.000000000000000000 ) ) ;
#1837 = CARTESIAN_POINT ( 'NONE',  ( 54.13287192849676188, 58.29948385550240175, 5.649768623646098220 ) ) ;
#1838 = CARTESIAN_POINT ( 'NONE',  ( 52.29715082351547295, 54.39948385550239607, 6.992620115222774047 ) ) ;
#1839 = ADVANCED_FACE ( 'NONE', ( #9600 ), #10702, .F. ) ;
#1840 = ORIENTED_EDGE ( 'NONE', *, *, #2185, .F. ) ;
#1841 = CARTESIAN_POINT ( 'NONE',  ( 56.66441430157296821, 52.09948385550240602, 2.141517661632100111 ) ) ;
#1842 = PRODUCT_RELATED_PRODUCT_CATEGORY ( 'part', '', ( #7778 ) ) ;
#1843 = VERTEX_POINT ( 'NONE', #2389 ) ;
#1844 = DIRECTION ( 'NONE',  ( -0.000000000000000000, -0.000000000000000000, -1.000000000000000000 ) ) ;
#1845 = ORIENTED_EDGE ( 'NONE', *, *, #11259, .F. ) ;
#1846 = AXIS2_PLACEMENT_3D ( 'NONE', #11714, #8479, #7506 ) ;
#1847 = CARTESIAN_POINT ( 'NONE',  ( 4.124214193018069352, 2.028338413290941222, 3.513185186763553514 ) ) ;
#1848 = CARTESIAN_POINT ( 'NONE',  ( 4.050536630291690088, -2.401306687817039265, 2.976670123173768445 ) ) ;
#1849 = CARTESIAN_POINT ( 'NONE',  ( 6.196878017913832970, -3.367876570272822168, -4.166666666666666963 ) ) ;
#1850 = CARTESIAN_POINT ( 'NONE',  ( 55.71335778527780036, 62.90051614449765083, -1.832500667257213056 ) ) ;
#1851 = CARTESIAN_POINT ( 'NONE',  ( 7.336184427528458230, 0.000000000000000000, -8.105212085995399107 ) ) ;
#1852 = CARTESIAN_POINT ( 'NONE',  ( 58.41169779390614281, 57.99948385550241170, -0.02388180880523160798 ) ) ;
#1853 = CARTESIAN_POINT ( 'NONE',  ( 47.74827507625478518, 60.59948385550239891, 7.007379884777227730 ) ) ;
#1854 = LINE ( 'NONE', #6168, #3384 ) ;
#1855 = CIRCLE ( 'NONE', #5189, 4.800000000000000711 ) ;
#1856 = CARTESIAN_POINT ( 'NONE',  ( 42.38452918213188525, 49.09948385550241312, -2.450534656007040013 ) ) ;
#1857 = VERTEX_POINT ( 'NONE', #5521 ) ;
#1858 = CIRCLE ( 'NONE', #5194, 2.200000000000001066 ) ;
#1859 = ORIENTED_EDGE ( 'NONE', *, *, #52, .F. ) ;
#1860 =( REPRESENTATION_RELATIONSHIP ('NONE','NONE', #5328, #11930 ) REPRESENTATION_RELATIONSHIP_WITH_TRANSFORMATION ( #13059 )SHAPE_REPRESENTATION_RELATIONSHIP( ) );
#1861 = ORIENTED_EDGE ( 'NONE', *, *, #216, .F. ) ;
#1862 = AXIS2_PLACEMENT_3D ( 'NONE', #11735, #5396, #4345 ) ;
#1863 = EDGE_CURVE ( 'NONE', #3871, #1171, #1405, .T. ) ;
#1864 = CARTESIAN_POINT ( 'NONE',  ( 54.77701766759913227, 44.74161735293615294, -5.000000000000010658 ) ) ;
#1866 = VECTOR ( 'NONE', #4768, 1000.000000000000000 ) ;
#1865 =( NAMED_UNIT ( * ) PLANE_ANGLE_UNIT ( ) SI_UNIT ( $, .RADIAN. ) );
#1867 = CARTESIAN_POINT ( 'NONE',  ( 1.498123826657866475, -5.075000000000000178, -9.000000000000000000 ) ) ;
#1868 = FACE_OUTER_BOUND ( 'NONE', #1808, .T. ) ;
#1869 = CARTESIAN_POINT ( 'NONE',  ( 1.390230914382191596, 4.043987460488659202, -3.502507215260488582 ) ) ;
#1870 = CARTESIAN_POINT ( 'NONE',  ( 44.28664221472220675, 65.09948385550239891, -1.832500667257165317 ) ) ;
#1871 = CARTESIAN_POINT ( 'NONE',  ( 56.66441430157294690, 54.90051614449765793, -2.141517661632166281 ) ) ;
#1872 = ADVANCED_FACE ( 'NONE', ( #320, #8767, #8699 ), #10632, .T. ) ;
#1873 = CARTESIAN_POINT ( 'NONE',  ( 56.79116909180259398, 61.20051614449766220, 4.963592699178938972 ) ) ;
#1874 = CARTESIAN_POINT ( 'NONE',  ( 3.951447005078451813, -1.347150628109131443, -3.500000000000000444 ) ) ;
#1875 = EDGE_CURVE ( 'NONE', #5652, #1304, #11701, .T. ) ;
#1876 = CARTESIAN_POINT ( 'NONE',  ( 52.62207051974829852, 48.60051614449766788, -7.992620115222797139 ) ) ;
#1877 = EDGE_CURVE ( 'NONE', #13576, #11319, #3241, .T. ) ;
#1879 = EDGE_LOOP ( 'NONE', ( #8930, #10856, #8607, #6643 ) ) ;
#1878 = VERTEX_POINT ( 'NONE', #5462 ) ;
#1880 = VECTOR ( 'NONE', #6757, 1000.000000000000000 ) ;
#1881 = EDGE_LOOP ( 'NONE', ( #12271, #2264, #5006, #277 ) ) ;
#1882 = ORIENTED_EDGE ( 'NONE', *, *, #8132, .F. ) ;
#1883 = FACE_BOUND ( 'NONE', #13295, .T. ) ;
#1884 = CARTESIAN_POINT ( 'NONE',  ( 0.000000000000000000, 4.330127018922190096, -2.500000000000006217 ) ) ;
#1885 = CARTESIAN_POINT ( 'NONE',  ( 2.449293598294706513E-15, -20.00000000000000000, 15.00000000000000355 ) ) ;
#1886 = SHAPE_DEFINITION_REPRESENTATION ( #13143, #5848 ) ;
#1887 = CARTESIAN_POINT ( 'NONE',  ( 44.03140696652192787, 61.19948385550239323, -4.306917132069425058 ) ) ;
#1888 = CARTESIAN_POINT ( 'NONE',  ( 44.03140696652193498, 61.19948385550240033, -4.306917132069424170 ) ) ;
#1889 = CARTESIAN_POINT ( 'NONE',  ( -4.000000000000000000, -2.309401076758512694, -3.433295621305382461 ) ) ;
#1890 = CARTESIAN_POINT ( 'NONE',  ( 4.175813232069146785, -2.061359961916366057, 3.570380186727398542 ) ) ;
#1891 = CARTESIAN_POINT ( 'NONE',  ( 53.49409602498213445, 45.00000000000000711, -6.629536405711814240 ) ) ;
#1892 = CARTESIAN_POINT ( 'NONE',  ( 44.05948171654945611, 48.20051614449764799, -4.345558710429044069 ) ) ;
#1893 = CARTESIAN_POINT ( 'NONE',  ( 51.92680522751233951, 55.59948385550240602, -6.007379884777223289 ) ) ;
#1894 = CARTESIAN_POINT ( 'NONE',  ( 8.500000000000000000, 5.773502691896261751, -2.749426538070115714E-16 ) ) ;
#1895 = VERTEX_POINT ( 'NONE', #7597 ) ;
#1896 = DIRECTION ( 'NONE',  ( -1.000000000000000000, 0.000000000000000000, 0.000000000000000000 ) ) ;
#1897 = ORIENTED_EDGE ( 'NONE', *, *, #7519, .T. ) ;
#1898 = ORIENTED_EDGE ( 'NONE', *, *, #13606, .F. ) ;
#1899 = DIRECTION ( 'NONE',  ( 1.000000000000000000, 0.000000000000000000, 0.000000000000000000 ) ) ;
#1900 = AXIS2_PLACEMENT_3D ( 'NONE', #913, #9299, #8403 ) ;
#1901 = PRODUCT_DEFINITION_SHAPE ( 'NONE', 'NONE',  #12904 ) ;
#1902 = EDGE_CURVE ( 'NONE', #3871, #1558, #8498, .T. ) ;
#1903 = FACE_OUTER_BOUND ( 'NONE', #3125, .T. ) ;
#1904 = SURFACE_SIDE_STYLE ('',( #11450 ) ) ;
#1905 = CARTESIAN_POINT ( 'NONE',  ( 62.49999999999998579, 5.000000000000018652, -5.000000000000000000 ) ) ;
#1906 =( LENGTH_UNIT ( ) NAMED_UNIT ( * ) SI_UNIT ( .MILLI., .METRE. ) );
#1907 = CARTESIAN_POINT ( 'NONE',  ( 3.309651814758564736, -5.455921364805393026, 0.000000000000000000 ) ) ;
#1908 = CARTESIAN_POINT ( 'NONE',  ( 43.69122665457040000, 46.00051614449764514, -0.02388180880515696977 ) ) ;
#1909 = CARTESIAN_POINT ( 'NONE',  ( -4.000000000000000000, -2.309401076758512694, -5.000000000000000000 ) ) ;
#1910 = CARTESIAN_POINT ( 'NONE',  ( 52.25172492374522903, 57.59948385550241312, -7.007379884777225953 ) ) ;
#1911 = CARTESIAN_POINT ( 'NONE',  ( 54.09612160359786515, 55.69948385550240744, -5.676469297603166098 ) ) ;
#1912 = VERTEX_POINT ( 'NONE', #8629 ) ;
#1913 = CARTESIAN_POINT ( 'NONE',  ( 43.33558569842703179, 49.09948385550240602, -2.141517661632099223 ) ) ;
#1914 = B_SPLINE_CURVE_WITH_KNOTS ( 'NONE', 3,
 ( #4422, #9543, #1359, #12843, #11880 ),
 .UNSPECIFIED., .F., .F.,
 ( 4, 1, 4 ),
 ( 0.000000000000000000, 0.002020725942163690940, 0.004041451884327382747 ),
 .UNSPECIFIED. ) ;
#1915 = VERTEX_POINT ( 'NONE', #2324 ) ;
#1916 = DIRECTION ( 'NONE',  ( -1.000000000000000000, 0.000000000000000000, 0.000000000000000000 ) ) ;
#1917 = ORIENTED_EDGE ( 'NONE', *, *, #7876, .T. ) ;
#1918 = DIRECTION ( 'NONE',  ( -1.000000000000000000, 0.000000000000000000, 0.000000000000000000 ) ) ;
#1919 = FACE_OUTER_BOUND ( 'NONE', #11842, .T. ) ;
#1920 = CARTESIAN_POINT ( 'NONE',  ( 3.973110223767137850, 2.263269463293572928E-11, 3.565797985667434222 ) ) ;
#1921 = CARTESIAN_POINT ( 'NONE',  ( 46.45491332379576477, 63.70051614449766930, 4.840751629271188961 ) ) ;
#1922 = CARTESIAN_POINT ( 'NONE',  ( -4.000000000000000000, 0.9868501483902560878, -0.09357334158579519445 ) ) ;
#1923 = CARTESIAN_POINT ( 'NONE',  ( 47.37792948025162332, 57.39948385550241028, -7.992620115222770494 ) ) ;
#1924 = CARTESIAN_POINT ( 'NONE',  ( -74.99999999999997158, 40.00000000000001421, 10.00000000000000000 ) ) ;
#1925 = CARTESIAN_POINT ( 'NONE',  ( 56.81924384183011512, 52.19948385550240744, 4.924951120819313743 ) ) ;
#1926 = ORIENTED_EDGE ( 'NONE', *, *, #13606, .T. ) ;
#1927 = EDGE_LOOP ( 'NONE', ( #10839, #7588, #9235, #5962 ) ) ;
#1928 = ORIENTED_EDGE ( 'NONE', *, *, #12695, .F. ) ;
#1929 = DIRECTION ( 'NONE',  ( 0.000000000000000000, 0.000000000000000000, 1.000000000000000000 ) ) ;
#1930 = VECTOR ( 'NONE', #7556, 1000.000000000000000 ) ;
#1931 =( LENGTH_UNIT ( ) NAMED_UNIT ( * ) SI_UNIT ( .MILLI., .METRE. ) );
#1932 = CARTESIAN_POINT ( 'NONE',  ( 1.925929944387235853E-31, 15.00000000000001599, 15.00000000000000000 ) ) ;
#1933 = CARTESIAN_POINT ( 'NONE',  ( -1.317756351988340180, 3.857995168970202116, -0.04852650426601388955 ) ) ;
#1934 = CARTESIAN_POINT ( 'NONE',  ( -0.02511973781850462134, 4.877415612947412882, -3.751298745799839462 ) ) ;
#1935 = CARTESIAN_POINT ( 'NONE',  ( 53.54508667620428497, 64.29948385550240175, 4.840751629271157874 ) ) ;
#1936 = CARTESIAN_POINT ( 'NONE',  ( 52.25172492374528588, 53.40051614449765083, 7.007379884777204637 ) ) ;
#1937 = ADVANCED_FACE ( 'NONE', ( #6562, #10762, #4278, #11609 ), #6367, .F. ) ;
#1938 = CARTESIAN_POINT ( 'NONE',  ( 41.58830220609386430, 62.00051614449766646, -0.02388180880514929535 ) ) ;
#1939 = CARTESIAN_POINT ( 'NONE',  ( 1.925929944387235853E-31, 15.00000000000001599, 9.999999999999998224 ) ) ;
#1940 = CARTESIAN_POINT ( 'NONE',  ( 45.31609314410960820, 52.30051614449766362, -6.485486291978072693 ) ) ;
#1942 = ORIENTED_EDGE ( 'NONE', *, *, #3391, .T. ) ;
#1941 = ORIENTED_EDGE ( 'NONE', *, *, #3233, .F. ) ;
#1943 = EDGE_LOOP ( 'NONE', ( #3043, #4233, #2144, #2017 ) ) ;
#1944 = UNCERTAINTY_MEASURE_WITH_UNIT (LENGTH_MEASURE( 1.000000000000000082E-05 ), #6590, 'distance_accuracy_value', 'NONE');
#1945 = ORIENTED_EDGE ( 'NONE', *, *, #9317, .T. ) ;
#1946 = EDGE_CURVE ( 'NONE', #2436, #11305, #3639, .T. ) ;
#1947 = CARTESIAN_POINT ( 'NONE',  ( 6.533910050139697390, 5.901028503456123175, 1.520834953648585461E-14 ) ) ;
#1948 = CARTESIAN_POINT ( 'NONE',  ( 6.534838248920897819, 2.951765777552411318, -5.112608298763837489 ) ) ;
#1949 = EDGE_CURVE ( 'NONE', #3416, #8098, #11368, .T. ) ;
#1950 = DIRECTION ( 'NONE',  ( 0.000000000000000000, 0.000000000000000000, -1.000000000000000000 ) ) ;
#1951 = CARTESIAN_POINT ( 'NONE',  ( 2.449293598294706513E-15, -20.00000000000000000, 9.000000000000000000 ) ) ;
#1952 = EDGE_CURVE ( 'NONE', #3196, #4232, #3412, .T. ) ;
#1953 = SHAPE_DEFINITION_REPRESENTATION ( #5881, #9196 ) ;
#1954 = CARTESIAN_POINT ( 'NONE',  ( 49.97728705011488159, 63.49948385550241170, -7.000000000000000888 ) ) ;
#1955 = CIRCLE ( 'NONE', #3499, 15.00000000000000000 ) ;
#1956 = CARTESIAN_POINT ( 'NONE',  ( 45.86712807150323812, 57.29948385550240175, -5.649768623646098220 ) ) ;
#1957 = CARTESIAN_POINT ( 'NONE',  ( 43.34962307344078880, 60.10051614449766078, -2.184720259617096705 ) ) ;
#1958 = CIRCLE ( 'NONE', #12979, 5.000000000000000000 ) ;
#1959 = DIRECTION ( 'NONE',  ( 0.000000000000000000, 0.000000000000000000, -1.000000000000000000 ) ) ;
#1960 = CARTESIAN_POINT ( 'NONE',  ( 2.449293598294706513E-15, -20.00000000000000000, 15.00000000000000355 ) ) ;
#1961 = CARTESIAN_POINT ( 'NONE',  ( 55.13865474201621453, 45.00000000000007816, -5.383573523308436748 ) ) ;
#1962 = CARTESIAN_POINT ( 'NONE',  ( 43.33558569842706021, 51.90051614449765793, 2.141517661632167169 ) ) ;
#1963 = CARTESIAN_POINT ( 'NONE',  ( 44.30067958973596376, 54.89948385550240317, 1.875703265242204099 ) ) ;
#1964 = DIRECTION ( 'NONE',  ( -1.000000000000000000, -0.000000000000000000, -0.000000000000000000 ) ) ;
#1965 = ORIENTED_EDGE ( 'NONE', *, *, #2820, .T. ) ;
#1966 = STYLED_ITEM ( 'NONE', ( #1341 ), #2368 ) ;
#1967 = DIRECTION ( 'NONE',  ( 0.000000000000000000, 0.000000000000000000, 1.000000000000000000 ) ) ;
#1968 = CIRCLE ( 'NONE', #5948, 1.500000000000000222 ) ;
#1969 = ORIENTED_EDGE ( 'NONE', *, *, #13348, .F. ) ;
#1970 = ORIENTED_EDGE ( 'NONE', *, *, #5773, .F. ) ;
#1971 = DIRECTION ( 'NONE',  ( 0.000000000000000000, 0.000000000000000000, 1.000000000000000000 ) ) ;
#1972 = AXIS2_PLACEMENT_3D ( 'NONE', #3079, #6284, #1896 ) ;
#1973 = DIRECTION ( 'NONE',  ( 0.000000000000000000, 0.000000000000000000, 1.000000000000000000 ) ) ;
#1974 = LINE ( 'NONE', #1830, #6444 ) ;
#1975 = DIRECTION ( 'NONE',  ( 1.000000000000000000, -6.938893903907227392E-16, 0.000000000000000000 ) ) ;
#1976 = CIRCLE ( 'NONE', #1516, 12.49999999999999645 ) ;
#1977 = CARTESIAN_POINT ( 'NONE',  ( 2.449293598294706513E-15, -20.00000000000000000, 15.00000000000000355 ) ) ;
#1978 = CARTESIAN_POINT ( 'NONE',  ( 44.30067958973594955, 48.10051614449766078, -1.875703265242155693 ) ) ;
#1979 = LINE ( 'NONE', #13648, #9822 ) ;
#1980 = CARTESIAN_POINT ( 'NONE',  ( 52.25172492374522903, 63.59948385550237759, -7.007379884777225953 ) ) ;
#1981 = CARTESIAN_POINT ( 'NONE',  ( 56.66441430157296821, 54.09948385550240602, 2.141517661632100111 ) ) ;
#1982 = COLOUR_RGB ( '',0.8941176470588234615, 0.8941176470588234615, 0.8941176470588234615 ) ;
#1983 = EDGE_LOOP ( 'NONE', ( #2851, #3400, #11674, #11892 ) ) ;
#1984 = CARTESIAN_POINT ( 'NONE',  ( 44.03140696652192787, 53.19948385550238612, -4.306917132069425058 ) ) ;
#1985 = EDGE_LOOP ( 'NONE', ( #12272, #3857 ) ) ;
#1986 = DIRECTION ( 'NONE',  ( 0.000000000000000000, 0.000000000000000000, 1.000000000000000000 ) ) ;
#1987 = FACE_OUTER_BOUND ( 'NONE', #1190, .T. ) ;
#1988 = AXIS2_PLACEMENT_3D ( 'NONE', #7337, #1012, #3309 ) ;
#1989 = ORIENTED_EDGE ( 'NONE', *, *, #11540, .T. ) ;
#1990 = CARTESIAN_POINT ( 'NONE',  ( -0.6666666666666666297, -4.233901974057276973, -3.300726591567087365 ) ) ;
#1991 = EDGE_CURVE ( 'NONE', #12658, #9525, #5931, .T. ) ;
#1992 = DIRECTION ( 'NONE',  ( 0.000000000000000000, -0.000000000000000000, 1.000000000000000000 ) ) ;
#1993 = PLANE ( 'NONE',  #11909 ) ;
#1994 = CARTESIAN_POINT ( 'NONE',  ( 42.63976443033212860, 48.00051614449766646, -0.02388180880514948964 ) ) ;
#1995 = DIRECTION ( 'NONE',  ( 1.000000000000000000, 3.469446951953615175E-16, 0.000000000000000000 ) ) ;
#1996 = CARTESIAN_POINT ( 'NONE',  ( 44.05948171654949874, 48.79948385550238754, 4.345558710429105354 ) ) ;
#1997 = CARTESIAN_POINT ( 'NONE',  ( 6.367873360227559232, -5.773502691896263528, 0.000000000000000000 ) ) ;
#1998 = VECTOR ( 'NONE', #268, 1000.000000000000114 ) ;
#1999 = DIRECTION ( 'NONE',  ( 0.000000000000000000, 0.000000000000000000, 1.000000000000000000 ) ) ;
#2000 = CARTESIAN_POINT ( 'NONE',  ( 47.37792948025162332, 49.39948385550241028, -7.992620115222770494 ) ) ;
#2001 = ORIENTED_EDGE ( 'NONE', *, *, #13529, .F. ) ;
#2002 = ORIENTED_EDGE ( 'NONE', *, *, #8419, .F. ) ;
#2003 = ORIENTED_EDGE ( 'NONE', *, *, #11505, .F. ) ;
#2004 = CARTESIAN_POINT ( 'NONE',  ( 5.599999999999999645, 2.020725942163686284, -3.499999999999999556 ) ) ;
#2005 = CIRCLE ( 'NONE', #867, 12.49999999999999645 ) ;
#2006 = FACE_OUTER_BOUND ( 'NONE', #758, .T. ) ;
#2007 = CARTESIAN_POINT ( 'NONE',  ( 6.095473853218515536, -4.853892138987517590, 1.592812200814445633 ) ) ;
#2008 = CARTESIAN_POINT ( 'NONE',  ( -0.1756481739660520902, 4.720212674038980261, -3.469390959564065291 ) ) ;
#2009 = CARTESIAN_POINT ( 'NONE',  ( 51.92680522751238925, 51.40051614449767214, 6.007379884777208190 ) ) ;
#2010 = CARTESIAN_POINT ( 'NONE',  ( 55.96859303347802239, 56.80051614449764941, -4.306917132069484566 ) ) ;
#2011 = CARTESIAN_POINT ( 'NONE',  ( 57.61547081786810764, 60.90051614449766504, -2.450534656007114176 ) ) ;
#2012 = CARTESIAN_POINT ( 'NONE',  ( 54.72065718078918906, 48.70051614449766930, -6.458785618021089192 ) ) ;
#2013 = EDGE_CURVE ( 'NONE', #5545, #4887, #2463, .T. ) ;
#2014 = PRODUCT_DEFINITION_SHAPE ( 'NONE', 'NONE',  #13676 ) ;
#2016 = ORIENTED_EDGE ( 'NONE', *, *, #10894, .F. ) ;
#2015 = ORIENTED_EDGE ( 'NONE', *, *, #2346, .F. ) ;
#2017 = ORIENTED_EDGE ( 'NONE', *, *, #7591, .T. ) ;
#2018 = VERTEX_POINT ( 'NONE', #5728 ) ;
#2019 = ADVANCED_FACE ( 'NONE', ( #9864 ), #6886, .T. ) ;
#2020 = DIRECTION ( 'NONE',  ( 0.9989677110047502362, 0.04542589977017699732, -6.931730960091013400E-15 ) ) ;
#2021 = DIRECTION ( 'NONE',  ( 0.000000000000000000, -0.4999999999999991118, 0.8660254037844391517 ) ) ;
#2022 = DIRECTION ( 'NONE',  ( 1.000000000000000000, 0.000000000000000000, 0.000000000000000000 ) ) ;
#2023 = AXIS2_PLACEMENT_3D ( 'NONE', #1951, #6398, #6196 ) ;
#2024 = CARTESIAN_POINT ( 'NONE',  ( 44.30067958973596376, 52.89948385550241028, 1.875703265242204099 ) ) ;
#2025 = AXIS2_PLACEMENT_3D ( 'NONE', #7469, #1153, #1282 ) ;
#2026 = CARTESIAN_POINT ( 'NONE',  ( 2.000000000000000000, 1.329782007511004727, -0.7677500000000018199 ) ) ;
#2027 = AXIS2_PLACEMENT_3D ( 'NONE', #6696, #5868, #10059 ) ;
#2028 = CARTESIAN_POINT ( 'NONE',  ( 44.05948171654945611, 58.20051614449764799, -4.345558710429044069 ) ) ;
#2029 = DIRECTION ( 'NONE',  ( 0.000000000000000000, 0.000000000000000000, -1.000000000000000000 ) ) ;
#2030 = DIRECTION ( 'NONE',  ( -1.000000000000000000, 0.000000000000000000, 0.000000000000000000 ) ) ;
#2031 = CARTESIAN_POINT ( 'NONE',  ( 4.033901012036086087, 3.740908793663944021, -0.5205559028925770271 ) ) ;
#2032 = CARTESIAN_POINT ( 'NONE',  ( 47.74827507625469281, 48.40051614449764372, -7.007379884777203749 ) ) ;
#2033 = CARTESIAN_POINT ( 'NONE',  ( 55.71335778527780747, 62.09948385550240602, 1.832500667257165983 ) ) ;
#2034 = CYLINDRICAL_SURFACE ( 'NONE', #5843, 4.800000000000000711 ) ;
#2035 = ORIENTED_EDGE ( 'NONE', *, *, #8494, .F. ) ;
#2036 = DIRECTION ( 'NONE',  ( 1.000000000000000000, 0.000000000000000000, 0.000000000000000000 ) ) ;
#2037 = EDGE_LOOP ( 'NONE', ( #1141, #13502, #3151, #1789, #6299, #5735, #9395 ) ) ;
#2038 = EDGE_LOOP ( 'NONE', ( #1928, #7008, #535, #8066, #1169, #11779 ) ) ;
#2039 = DIRECTION ( 'NONE',  ( 0.000000000000000000, 1.000000000000000000, 0.000000000000000000 ) ) ;
#2040 = LINE ( 'NONE', #991, #13547 ) ;
#2041 = ADVANCED_FACE ( 'NONE', ( #5797, #448 ), #4685, .F. ) ;
#2042 = CYLINDRICAL_SURFACE ( 'NONE', #21, 4.799999999999999822 ) ;
#2043 =( NAMED_UNIT ( * ) SI_UNIT ( $, .STERADIAN. ) SOLID_ANGLE_UNIT ( ) );
#2044 = CARTESIAN_POINT ( 'NONE',  ( 0.4465819873852039379, 5.773502691896261751, 3.331019006688249527E-17 ) ) ;
#2045 = CARTESIAN_POINT ( 'NONE',  ( 55.69932041026405045, 53.10051614449767499, 1.875703265242156359 ) ) ;
#2046 = CARTESIAN_POINT ( 'NONE',  ( 5.991014884144047592, -4.330127018922191873, 2.499999999999998668 ) ) ;
#2047 = CARTESIAN_POINT ( 'NONE',  ( 54.09612160359786515, 63.69948385550240744, -5.676469297603166098 ) ) ;
#2048 = CARTESIAN_POINT ( 'NONE',  ( 57.36023556966787851, 55.99948385550239038, -0.02388180880522424582 ) ) ;
#2049 = AXIS2_PLACEMENT_3D ( 'NONE', #4295, #11820, #3393 ) ;
#2050 = ORIENTED_EDGE ( 'NONE', *, *, #13637, .T. ) ;
#2051 = EDGE_CURVE ( 'NONE', #11355, #9438, #7121, .T. ) ;
#2052 = ADVANCED_FACE ( 'NONE', ( #9106 ), #3508, .T. ) ;
#2053 = AXIS2_PLACEMENT_3D ( 'NONE', #7555, #1172, #5423 ) ;
#2054 = EDGE_LOOP ( 'NONE', ( #807, #5754, #11148, #12724 ) ) ;
#2055 = FACE_OUTER_BOUND ( 'NONE', #4086, .T. ) ;
#2056 = ADVANCED_FACE ( 'NONE', ( #9033 ), #8656, .F. ) ;
#2057 = CARTESIAN_POINT ( 'NONE',  ( -74.99999999999997158, 40.00000000000001421, 5.000000000000018652 ) ) ;
#2058 = CARTESIAN_POINT ( 'NONE',  ( -2.687328764639638656, 3.067272167851286202, -0.05923475698270370959 ) ) ;
#2059 = LINE ( 'NONE', #9190, #7185 ) ;
#2060 = CARTESIAN_POINT ( 'NONE',  ( 52.29715082351547295, 48.39948385550240317, 6.992620115222774047 ) ) ;
#2061 = B_SPLINE_CURVE_WITH_KNOTS ( 'NONE', 3,
 ( #7643, #2237, #2168, #11847 ),
 .UNSPECIFIED., .F., .F.,
 ( 4, 4 ),
 ( 2.380735200831979558E-07, 0.002921158011986727237 ),
 .UNSPECIFIED. ) ;
#2062 = CARTESIAN_POINT ( 'NONE',  ( 45.86712807150329496, 47.70051614449766220, 5.649768623646139964 ) ) ;
#2063 = CARTESIAN_POINT ( 'NONE',  ( 2.000000000000000000, 0.8865213383406680414, -1.535500000000000975 ) ) ;
#2064 = CARTESIAN_POINT ( 'NONE',  ( 45.86712807150323812, 47.29948385550240886, -5.649768623646098220 ) ) ;
#2065 = CARTESIAN_POINT ( 'NONE',  ( 15.00000000000000355, -19.99999999999984368, -9.000000000000000000 ) ) ;
#2066 = CARTESIAN_POINT ( 'NONE',  ( 47.37792948025162332, 55.39948385550240317, -7.992620115222770494 ) ) ;
#2067 = VERTEX_POINT ( 'NONE', #10893 ) ;
#2068 = EDGE_LOOP ( 'NONE', ( #13556, #11987 ) ) ;
#2069 = CARTESIAN_POINT ( 'NONE',  ( -2.649999999999988365, 15.00000000000001599, 9.999999999999998224 ) ) ;
#2070 = CARTESIAN_POINT ( 'NONE',  ( -0.9999999999999995559, -15.10102051443364246, 15.00000000000000355 ) ) ;
#2071 = CARTESIAN_POINT ( 'NONE',  ( 6.244889965166096069, -3.924082311521025712, -3.413878157001049907 ) ) ;
#2072 = CARTESIAN_POINT ( 'NONE',  ( 4.140404888673277384, 2.228338276487440428, -3.686887068327033390 ) ) ;
#2073 = CARTESIAN_POINT ( 'NONE',  ( 53.54508667620424234, 50.70051614449766220, -4.840751629271188961 ) ) ;
#2074 = CARTESIAN_POINT ( 'NONE',  ( 50.02271294988505446, 58.50051614449765935, -7.000000000000000888 ) ) ;
#2075 = AXIS2_PLACEMENT_3D ( 'NONE', #11915, #13080, #3485 ) ;
#2076 = CARTESIAN_POINT ( 'NONE',  ( 43.20883090819742023, 64.20051614449766930, -4.963592699178938972 ) ) ;
#2077 = CARTESIAN_POINT ( 'NONE',  ( -4.000000000000000000, -2.512220745329312610, -3.469390707569719901 ) ) ;
#2078 = AXIS2_PLACEMENT_3D ( 'NONE', #6069, #8129, #1606 ) ;
#2079 = CARTESIAN_POINT ( 'NONE',  ( 42.39856655714564226, 56.10051614449766078, -2.493737253992044156 ) ) ;
#2080 = ORIENTED_EDGE ( 'NONE', *, *, #227, .T. ) ;
#2081 = EDGE_CURVE ( 'NONE', #10697, #3166, #4244, .T. ) ;
#2082 = ORIENTED_EDGE ( 'NONE', *, *, #10013, .T. ) ;
#2083 = ORIENTED_EDGE ( 'NONE', *, *, #11849, .F. ) ;
#2084 = CIRCLE ( 'NONE', #4091, 5.000000000000000000 ) ;
#2085 = FACE_OUTER_BOUND ( 'NONE', #6497, .T. ) ;
#2086 = FILL_AREA_STYLE ('',( #7363 ) ) ;
#2087 = DIRECTION ( 'NONE',  ( 1.000000000000000000, 0.000000000000000000, 0.000000000000000000 ) ) ;
#2088 = AXIS2_PLACEMENT_3D ( 'NONE', #10550, #3091, #790 ) ;
#2089 = CARTESIAN_POINT ( 'NONE',  ( -4.154094228333736538, -2.398367420967545627, -3.721909803043222276 ) ) ;
#2090 = CARTESIAN_POINT ( 'NONE',  ( 44.30067958973596376, 48.89948385550241028, 1.875703265242204099 ) ) ;
#2091 = LINE ( 'NONE', #6336, #7295 ) ;
#2092 = CARTESIAN_POINT ( 'NONE',  ( 56.79116909180259398, 47.20051614449766220, 4.963592699178938972 ) ) ;
#2093 = CARTESIAN_POINT ( 'NONE',  ( -75.00000000000001421, 4.999999999999974243, 0.000000000000000000 ) ) ;
#2094 = LINE ( 'NONE', #8465, #1009 ) ;
#2095 = CARTESIAN_POINT ( 'NONE',  ( 3.948103430091020272, 2.682758828852976229, -2.353325403973173024 ) ) ;
#2096 = CARTESIAN_POINT ( 'NONE',  ( 56.65037692655921120, 53.10051614449766078, 2.184720259617097593 ) ) ;
#2097 = CARTESIAN_POINT ( 'NONE',  ( 46.49166364869460466, 58.69948385550240033, 4.867452303228209765 ) ) ;
#2098 = CARTESIAN_POINT ( 'NONE',  ( 1.267864665261691752E-11, -20.00000000000000000, 9.999999999999998224 ) ) ;
#2099 = B_SPLINE_CURVE_WITH_KNOTS ( 'NONE', 3,
 ( #2612, #1849, #1565, #11115, #11326 ),
 .UNSPECIFIED., .F., .F.,
 ( 4, 1, 4 ),
 ( 0.000000000000000000, 0.002886751345948128985, 0.005773502691896257970 ),
 .UNSPECIFIED. ) ;
#2100 = ORIENTED_EDGE ( 'NONE', *, *, #8511, .F. ) ;
#2101 = CARTESIAN_POINT ( 'NONE',  ( 53.50000000000000000, 0.000000000000000000, 0.000000000000000000 ) ) ;
#2102 = VERTEX_POINT ( 'NONE', #1413 ) ;
#2103 = CARTESIAN_POINT ( 'NONE',  ( 0.3126073911696427010, 4.041451884327382338, -6.521455134176256610E-17 ) ) ;
#2104 = DIRECTION ( 'NONE',  ( 0.000000000000000000, 0.000000000000000000, -1.000000000000000000 ) ) ;
#2105 = CARTESIAN_POINT ( 'NONE',  ( 6.095484975317565279, -1.047622383848427985, 4.999999999999999112 ) ) ;
#2106 = CARTESIAN_POINT ( 'NONE',  ( 47.74827507625478518, 50.59948385550238470, 7.007379884777227730 ) ) ;
#2107 = DIRECTION ( 'NONE',  ( -1.000000000000000000, 0.000000000000000000, 0.000000000000000000 ) ) ;
#2108 = CARTESIAN_POINT ( 'NONE',  ( 55.11794222512599362, 48.80051614449767072, -3.688883143319583446 ) ) ;
#2109 = EDGE_CURVE ( 'NONE', #10425, #12479, #6894, .T. ) ;
#2110 = LINE ( 'NONE', #6358, #6956 ) ;
#2111 = CARTESIAN_POINT ( 'NONE',  ( 0.000000000000000000, 40.00000000000001421, -9.999999999999998224 ) ) ;
#2112 = CARTESIAN_POINT ( 'NONE',  ( 47.74827507625478518, 62.59948385550240602, 7.007379884777227730 ) ) ;
#2113 = CARTESIAN_POINT ( 'NONE',  ( 55.96859303347804371, 62.19948385550240744, 4.306917132069425946 ) ) ;
#2114 = ORIENTED_EDGE ( 'NONE', *, *, #2820, .F. ) ;
#2115 = VECTOR ( 'NONE', #8203, 1000.000000000000000 ) ;
#2116 = VERTEX_POINT ( 'NONE', #1548 ) ;
#2117 = DIRECTION ( 'NONE',  ( 0.000000000000000000, 0.000000000000000000, 1.000000000000000000 ) ) ;
#2118 = EDGE_CURVE ( 'NONE', #2448, #5823, #7733, .T. ) ;
#2119 = CARTESIAN_POINT ( 'NONE',  ( 0.000000000000000000, 0.000000000000000000, 10.00000000000000000 ) ) ;
#2120 = CARTESIAN_POINT ( 'NONE',  ( 3.878096787214416530, -2.680238624820946214, 2.357690525401583415 ) ) ;
#2121 = DIRECTION ( 'NONE',  ( -0.9989677110047502362, -0.04542589977017699732, 6.931730960091013400E-15 ) ) ;
#2122 = EDGE_CURVE ( 'NONE', #3926, #3999, #2684, .T. ) ;
#2123 = CARTESIAN_POINT ( 'NONE',  ( 43.33558569842703179, 47.09948385550240602, -2.141517661632099223 ) ) ;
#2124 = APPLICATION_CONTEXT ( 'automotive_design' ) ;
#2125 = CARTESIAN_POINT ( 'NONE',  ( 54.09612160359792199, 45.30051614449766362, 5.676469297603124353 ) ) ;
#2126 = EDGE_CURVE ( 'NONE', #1050, #2821, #12187, .T. ) ;
#2127 = CARTESIAN_POINT ( 'NONE',  ( 1.250000000000000000, -6.429618962271402616, -1.000000000000000000 ) ) ;
#2128 = CARTESIAN_POINT ( 'NONE',  ( 50.02271294988513972, 64.49948385550239038, 8.000000000000001776 ) ) ;
#2129 = CIRCLE ( 'NONE', #5675, 2.500000000000000888 ) ;
#2130 = DIRECTION ( 'NONE',  ( 0.000000000000000000, 0.000000000000000000, 1.000000000000000000 ) ) ;
#2131 = CARTESIAN_POINT ( 'NONE',  ( 56.81924384183011512, 58.19948385550240744, 4.924951120819313743 ) ) ;
#2132 = ORIENTED_EDGE ( 'NONE', *, *, #197, .F. ) ;
#2133 = ORIENTED_EDGE ( 'NONE', *, *, #1753, .F. ) ;
#2134 = CARTESIAN_POINT ( 'NONE',  ( 2.899426713160750069, -23.82535289025860337, -8.999999999999996447 ) ) ;
#2135 = CYLINDRICAL_SURFACE ( 'NONE', #3362, 2.649999999999985700 ) ;
#2136 = CARTESIAN_POINT ( 'NONE',  ( 6.212068001624178493, -5.350125758160219291, 0.7333103599835463227 ) ) ;
#2137 = DIRECTION ( 'NONE',  ( 0.000000000000000000, -1.000000000000000000, 9.783878858594328898E-16 ) ) ;
#2138 = CARTESIAN_POINT ( 'NONE',  ( 53.50833635130544508, 47.30051614449766362, 4.867452303228181343 ) ) ;
#2139 = EDGE_CURVE ( 'NONE', #13432, #2696, #4430, .T. ) ;
#2140 = CARTESIAN_POINT ( 'NONE',  ( 43.34962307344078880, 58.10051614449766078, -2.184720259617096705 ) ) ;
#2141 = CARTESIAN_POINT ( 'NONE',  ( 54.68390685589033495, 49.69948385550240744, -6.485486291978119766 ) ) ;
#2142 = CARTESIAN_POINT ( 'NONE',  ( 4.165266963751724560, -4.099263933823990236, 4.401844587977598791E-16 ) ) ;
#2143 = CARTESIAN_POINT ( 'NONE',  ( 49.97728705011495265, 55.50051614449766646, 8.000000000000001776 ) ) ;
#2144 = ORIENTED_EDGE ( 'NONE', *, *, #4008, .T. ) ;
#2145 = ORIENTED_EDGE ( 'NONE', *, *, #10169, .F. ) ;
#2146 = EDGE_LOOP ( 'NONE', ( #2804, #4087, #1578, #12361 ) ) ;
#2147 = CARTESIAN_POINT ( 'NONE',  ( -3.264650091097280831E-13, -4.796980096169642493, -3.721999068284424617 ) ) ;
#2148 = CARTESIAN_POINT ( 'NONE',  ( 6.533910050139693837, 2.950514251728067361, -5.110440592449059238 ) ) ;
#2149 = CARTESIAN_POINT ( 'NONE',  ( 2.449293598294706513E-15, -20.00000000000000000, 9.000000000000000000 ) ) ;
#2150 = CARTESIAN_POINT ( 'NONE',  ( 0.4465819873852006072, 2.886751345948123770, -5.000000000000000000 ) ) ;
#2151 = EDGE_CURVE ( 'NONE', #10268, #4104, #8551, .T. ) ;
#2152 = DIRECTION ( 'NONE',  ( -0.000000000000000000, -0.000000000000000000, -1.000000000000000000 ) ) ;
#2153 = CARTESIAN_POINT ( 'NONE',  ( 43.69122665457040000, 46.99948385550239749, 0.02388180880521036456 ) ) ;
#2154 = EDGE_CURVE ( 'NONE', #13341, #13443, #7780, .T. ) ;
#2155 = CARTESIAN_POINT ( 'NONE',  ( 55.96859303347805081, 64.19948385550239323, 4.306917132069425058 ) ) ;
#2156 = CARTESIAN_POINT ( 'NONE',  ( 52.62207051974829852, 46.60051614449764656, -7.992620115222797139 ) ) ;
#2157 = AXIS2_PLACEMENT_3D ( 'NONE', #5156, #6268, #4235 ) ;
#2158 = CARTESIAN_POINT ( 'NONE',  ( 0.1999999999999987899, 0.000000000000000000, 3.500000000000000000 ) ) ;
#2159 = FACE_OUTER_BOUND ( 'NONE', #4630, .T. ) ;
#2160 = CARTESIAN_POINT ( 'NONE',  ( 56.66441430157294690, 58.90051614449766504, -2.141517661632166281 ) ) ;
#2161 = CARTESIAN_POINT ( 'NONE',  ( 43.69122665457040000, 60.99948385550241170, 0.02388180880521036456 ) ) ;
#2162 = CARTESIAN_POINT ( 'NONE',  ( 55.41777406314699306, 44.91366546079681399, -4.999999999999999112 ) ) ;
#2163 = VERTEX_POINT ( 'NONE', #5576 ) ;
#2164 = DIRECTION ( 'NONE',  ( 0.000000000000000000, 1.000000000000000000, 0.000000000000000000 ) ) ;
#2165 = EDGE_LOOP ( 'NONE', ( #7409, #4103 ) ) ;
#2166 = CARTESIAN_POINT ( 'NONE',  ( 1.567478505476134606E-15, 4.618802153517012066, -5.000000000000000000 ) ) ;
#2167 = CONICAL_SURFACE ( 'NONE', #394, 5.000000000000000000, 1.047197551196600296 ) ;
#2168 = CARTESIAN_POINT ( 'NONE',  ( -3.917148844556152511E-15, -4.821944789745365334, 1.648146632869001094 ) ) ;
#2169 = FACE_OUTER_BOUND ( 'NONE', #7043, .T. ) ;
#2170 = TOROIDAL_SURFACE ( 'NONE', #5722, 2.200000000000001066, 0.2000000000000000111 ) ;
#2171 = SURFACE_STYLE_USAGE ( .BOTH. , #11851 ) ;
#2172 = CARTESIAN_POINT ( 'NONE',  ( 56.65037692655918988, 53.89948385550240317, -2.184720259617163762 ) ) ;
#2173 = DIRECTION ( 'NONE',  ( -0.000000000000000000, -0.000000000000000000, -1.000000000000000000 ) ) ;
#2174 = CARTESIAN_POINT ( 'NONE',  ( 55.71335778527780036, 50.90051614449765793, -1.832500667257213056 ) ) ;
#2175 = DIRECTION ( 'NONE',  ( 1.000000000000000000, 0.000000000000000000, -0.000000000000000000 ) ) ;
#2176 = CARTESIAN_POINT ( 'NONE',  ( 42.63976443033212860, 64.99948385550240459, 0.02388180880522514787 ) ) ;
#2177 = SURFACE_SIDE_STYLE ('',( #3231 ) ) ;
#2178 = CARTESIAN_POINT ( 'NONE',  ( 54.13287192849676188, 60.29948385550240886, 5.649768623646098220 ) ) ;
#2179 = CIRCLE ( 'NONE', #3511, 12.50000000000000000 ) ;
#2180 = EDGE_CURVE ( 'NONE', #10373, #4052, #370, .T. ) ;
#2181 = EDGE_LOOP ( 'NONE', ( #3330, #12040, #2890, #2015 ) ) ;
#2182 = AXIS2_PLACEMENT_3D ( 'NONE', #12816, #8688, #1396 ) ;
#2183 = ORIENTED_EDGE ( 'NONE', *, *, #4506, .T. ) ;
#2184 = CARTESIAN_POINT ( 'NONE',  ( -2.756197834950067094, -3.027510591568735254, -3.223146290109809797 ) ) ;
#2185 = EDGE_CURVE ( 'NONE', #1787, #12223, #12747, .T. ) ;
#2186 = LINE ( 'NONE', #6431, #12253 ) ;
#2187 = MECHANICAL_DESIGN_GEOMETRIC_PRESENTATION_REPRESENTATION (  '', ( #4406 ), #1286 ) ;
#2188 = FACE_OUTER_BOUND ( 'NONE', #13311, .T. ) ;
#2189 = CARTESIAN_POINT ( 'NONE',  ( 1.925929944387235853E-31, 15.00000000000001599, -9.000000000000000000 ) ) ;
#2190 = CARTESIAN_POINT ( 'NONE',  ( 45.90387839640214196, 52.69948385550240033, 5.676469297603166098 ) ) ;
#2191 = CARTESIAN_POINT ( 'NONE',  ( 43.33558569842706021, 45.90051614449765793, 2.141517661632167169 ) ) ;
#2192 = DIRECTION ( 'NONE',  ( -1.000000000000000000, 0.000000000000000000, -0.000000000000000000 ) ) ;
#2193 = CARTESIAN_POINT ( 'NONE',  ( 50.02271294988512551, 46.49948385550240459, 7.000000000000000888 ) ) ;
#2194 = SURFACE_STYLE_FILL_AREA ( #6636 ) ;
#2195 = CARTESIAN_POINT ( 'NONE',  ( 0.2499999999999966416, -8.096141056083448362, 0.000000000000000000 ) ) ;
#2196 = CARTESIAN_POINT ( 'NONE',  ( 52.62207051974839089, 54.39948385550241028, 7.992620115222770494 ) ) ;
#2197 = AXIS2_PLACEMENT_3D ( 'NONE', #5465, #11941, #6634 ) ;
#2198 = ORIENTED_EDGE ( 'NONE', *, *, #11069, .F. ) ;
#2199 = EDGE_LOOP ( 'NONE', ( #1525, #5702, #7813, #5010 ) ) ;
#2200 = LINE ( 'NONE', #3522, #6526 ) ;
#2201 = CARTESIAN_POINT ( 'NONE',  ( 6.357976367241810145, -3.426708043488799760, 4.282301071214263288 ) ) ;
#2202 = CARTESIAN_POINT ( 'NONE',  ( 8.759913291900311094, -7.823632761846075923, 0.000000000000000000 ) ) ;
#2203 = TOROIDAL_SURFACE ( 'NONE', #11708, 2.200000000000001066, 0.2000000000000000111 ) ;
#2204 = CARTESIAN_POINT ( 'NONE',  ( 51.97223112728249816, 46.60051614449764656, -5.992620115222793586 ) ) ;
#2205 = CARTESIAN_POINT ( 'NONE',  ( 56.65037692655921120, 61.10051614449766078, 2.184720259617097593 ) ) ;
#2206 = CARTESIAN_POINT ( 'NONE',  ( 56.81924384183006538, 62.80051614449766362, -4.924951120819380357 ) ) ;
#2207 = CARTESIAN_POINT ( 'NONE',  ( 4.180345304246197990, 4.135116856707394817, -0.02129519942689619277 ) ) ;
#2208 = CARTESIAN_POINT ( 'NONE',  ( 43.20883090819742023, 56.20051614449766220, -4.963592699178938972 ) ) ;
#2209 = ORIENTED_EDGE ( 'NONE', *, *, #3320, .F. ) ;
#2210 = EDGE_CURVE ( 'NONE', #10214, #2490, #3793, .T. ) ;
#2211 = ORIENTED_EDGE ( 'NONE', *, *, #1613, .T. ) ;
#2212 = EDGE_CURVE ( 'NONE', #6833, #12476, #6611, .T. ) ;
#2213 = ORIENTED_EDGE ( 'NONE', *, *, #3661, .T. ) ;
#2214 = AXIS2_PLACEMENT_3D ( 'NONE', #10842, #9748, #7676 ) ;
#2215 = CARTESIAN_POINT ( 'NONE',  ( 1.925929944387235853E-31, 15.00000000000001599, 15.00000000000000000 ) ) ;
#2216 = DIRECTION ( 'NONE',  ( 1.000000000000000000, 0.000000000000000000, 0.000000000000000000 ) ) ;
#2217 = ADVANCED_FACE ( 'NONE', ( #10689 ), #8818, .F. ) ;
#2218 = LINE ( 'NONE', #3202, #2513 ) ;
#2219 = CARTESIAN_POINT ( 'NONE',  ( 62.49999999999998579, 45.00000000000001421, -9.999999999999998224 ) ) ;
#2220 = FILL_AREA_STYLE ('',( #11697 ) ) ;
#2221 = CARTESIAN_POINT ( 'NONE',  ( 43.69122665457040000, 50.99948385550241170, 0.02388180880521036456 ) ) ;
#2222 = CARTESIAN_POINT ( 'NONE',  ( -74.99999999999997158, 32.50000000000001421, -15.00000000000000000 ) ) ;
#2223 = CARTESIAN_POINT ( 'NONE',  ( 50.02271294988505446, 64.50051614449765225, -7.000000000000000888 ) ) ;
#2224 = AXIS2_PLACEMENT_3D ( 'NONE', #5376, #10683, #37 ) ;
#2225 = CARTESIAN_POINT ( 'NONE',  ( 17.85000000000000142, -20.00000000000000000, -23.00000000000000000 ) ) ;
#2226 = DIRECTION ( 'NONE',  ( 1.000000000000000000, 0.000000000000000000, 0.000000000000000000 ) ) ;
#2227 = CARTESIAN_POINT ( 'NONE',  ( 44.03140696652198471, 57.80051614449766362, 4.306917132069485454 ) ) ;
#2228 = CARTESIAN_POINT ( 'NONE',  ( 48.07319477248768180, 58.59948385550239891, 6.007379884777225953 ) ) ;
#2229 = LINE ( 'NONE', #6473, #11363 ) ;
#2230 = ORIENTED_EDGE ( 'NONE', *, *, #7281, .T. ) ;
#2231 = DIRECTION ( 'NONE',  ( 0.000000000000000000, 0.000000000000000000, -1.000000000000000000 ) ) ;
#2232 = ORIENTED_EDGE ( 'NONE', *, *, #840, .T. ) ;
#2233 = CARTESIAN_POINT ( 'NONE',  ( 14.14213562373095101, -25.00000000000000711, -23.00000000000000000 ) ) ;
#2234 = AXIS2_PLACEMENT_3D ( 'NONE', #7626, #8735, #6727 ) ;
#2235 = PRODUCT ( 'idle-roller mover', 'idle-roller mover', '', ( #2933 ) ) ;
#2236 = AXIS2_PLACEMENT_3D ( 'NONE', #9076, #547, #4862 ) ;
#2237 = CARTESIAN_POINT ( 'NONE',  ( 0.1739375980333740523, -5.301268757141563093, 0.8179331680533010740 ) ) ;
#2238 = CARTESIAN_POINT ( 'NONE',  ( 56.65037692655918988, 49.89948385550240317, -2.184720259617163762 ) ) ;
#2239 = ADVANCED_FACE ( 'NONE', ( #5510 ), #12815, .F. ) ;
#2240 = DIRECTION ( 'NONE',  ( 0.000000000000000000, 0.000000000000000000, -1.000000000000000000 ) ) ;
#2241 = CARTESIAN_POINT ( 'NONE',  ( 56.30877334542961421, 51.00051614449765935, 0.02388180880515774693 ) ) ;
#2242 = DIRECTION ( 'NONE',  ( -1.000000000000000000, 0.000000000000000000, 0.000000000000000000 ) ) ;
#2243 = CARTESIAN_POINT ( 'NONE',  ( 44.05948171654949874, 64.79948385550240175, 4.345558710429105354 ) ) ;
#2244 = CARTESIAN_POINT ( 'NONE',  ( 54.13287192849676188, 58.29948385550240175, 5.649768623646098220 ) ) ;
#2245 = DIRECTION ( 'NONE',  ( 0.000000000000000000, 1.000000000000000000, -1.073081856240829552E-16 ) ) ;
#2246 = AXIS2_PLACEMENT_3D ( 'NONE', #4313, #5295, #10464 ) ;
#2247 = ORIENTED_EDGE ( 'NONE', *, *, #7828, .F. ) ;
#2248 = ORIENTED_EDGE ( 'NONE', *, *, #7970, .F. ) ;
#2249 = VERTEX_POINT ( 'NONE', #10812 ) ;
#2250 = CARTESIAN_POINT ( 'NONE',  ( -3.472371940586054251, -2.614027278893156669, -3.320322319202162031 ) ) ;
#2251 = CARTESIAN_POINT ( 'NONE',  ( 0.1983443223721553794, -3.359771601077102154, 4.180704885107414448 ) ) ;
#2252 = CARTESIAN_POINT ( 'NONE',  ( 3.948103430090711630, -2.682758828852738642, 2.353325403972896357 ) ) ;
#2253 = DIRECTION ( 'NONE',  ( -0.000000000000000000, -1.000000000000000000, -0.000000000000000000 ) ) ;
#2254 = CARTESIAN_POINT ( 'NONE',  ( 47.74827507625477807, 54.59948385550239891, 7.007379884777229506 ) ) ;
#2255 = AXIS2_PLACEMENT_3D ( 'NONE', #1939, #13474, #1803 ) ;
#2256 = CARTESIAN_POINT ( 'NONE',  ( 42.63976443033212860, 54.00051614449766646, -0.02388180880514948964 ) ) ;
#2257 = EDGE_CURVE ( 'NONE', #1320, #10476, #11856, .T. ) ;
#2258 = CARTESIAN_POINT ( 'NONE',  ( 0.3126073911696399255, 2.020725942163686284, -3.499999999999999556 ) ) ;
#2259 = CARTESIAN_POINT ( 'NONE',  ( 47.74827507625478518, 48.59948385550239180, 7.007379884777227730 ) ) ;
#2260 =( NAMED_UNIT ( * ) PLANE_ANGLE_UNIT ( ) SI_UNIT ( $, .RADIAN. ) );
#2261 = PRODUCT_RELATED_PRODUCT_CATEGORY ( 'part', '', ( #13599 ) ) ;
#2262 = CARTESIAN_POINT ( 'NONE',  ( 54.72065718078924590, 54.29948385550241596, 6.458785618021043895 ) ) ;
#2263 = EDGE_LOOP ( 'NONE', ( #13482, #7170, #7393, #11395, #11422 ) ) ;
#2264 = ORIENTED_EDGE ( 'NONE', *, *, #1549, .T. ) ;
#2265 = B_SPLINE_CURVE_WITH_KNOTS ( 'NONE', 3,
 ( #1593, #2787, #4941, #7007, #11213, #13344, #7975, #12190 ),
 .UNSPECIFIED., .F., .F.,
 ( 4, 2, 2, 4 ),
 ( 2.465131517075058656E-07, 0.001183067374689851080, 0.001774477805458923299, 0.002365888236227995517 ),
 .UNSPECIFIED. ) ;
#2266 = DIRECTION ( 'NONE',  ( -0.9768494444668812671, -0.2139279384389642935, 0.000000000000000000 ) ) ;
#2267 = CARTESIAN_POINT ( 'NONE',  ( -1.000000000000000000, -14.00000000000000000, 8.999999999999998224 ) ) ;
#2268 =( GEOMETRIC_REPRESENTATION_CONTEXT ( 3 ) GLOBAL_UNCERTAINTY_ASSIGNED_CONTEXT ( ( #7859 ) ) GLOBAL_UNIT_ASSIGNED_CONTEXT ( ( #1906, #3270, #9695 ) ) REPRESENTATION_CONTEXT ( 'NONE', 'WORKASPACE' ) );
#2269 = CARTESIAN_POINT ( 'NONE',  ( 55.11794222512599362, 50.80051614449766362, -3.688883143319583446 ) ) ;
#2270 = CARTESIAN_POINT ( 'NONE',  ( 45.90387839640208512, 62.30051614449766362, -5.676469297603124353 ) ) ;
#2271 =( BOUNDED_SURFACE ( )  B_SPLINE_SURFACE ( 3, 2, ( 
 ( #7306, #11514, #13632 ),
 ( #4181, #2031, #8404 ),
 ( #12609, #3142, #7372 ),
 ( #11581, #2095, #2842 ),
 ( #12443, #7207, #1581 ),
 ( #1652, #11274, #541 ) ),
 .UNSPECIFIED., .F., .F., .F. ) 
 B_SPLINE_SURFACE_WITH_KNOTS ( ( 4, 2, 4 ),
 ( 3, 3 ),
 ( 0.01651999345535503164, 0.01858032176739832925, 0.02064065007944162339 ),
 ( 0.000000000000000000, 1.000000000000000000 ),
 .UNSPECIFIED. ) 
 GEOMETRIC_REPRESENTATION_ITEM ( )  RATIONAL_B_SPLINE_SURFACE ( (
 ( 1.000000000000000000, 0.8047781103519391355, 1.000000000000000000),
 ( 1.000000000000000000, 0.8123785825612301892, 1.000000000000000000),
 ( 1.000000000000000000, 0.8190671539777686361, 1.000000000000000000),
 ( 1.000000000000000000, 0.8192352254845479687, 1.000000000000000000),
 ( 1.000000000000000000, 0.8126129677203643986, 1.000000000000000000),
 ( 1.000000000000000000, 0.8047712537969725632, 1.000000000000000000) ) ) 
 REPRESENTATION_ITEM ( '' )  SURFACE ( )  );
#2272 = CARTESIAN_POINT ( 'NONE',  ( 50.02271294988513972, 48.49948385550241170, 8.000000000000001776 ) ) ;
#2273 = CARTESIAN_POINT ( 'NONE',  ( 3.880206590543030742, 2.665671387532550618, 2.382921720510995822 ) ) ;
#2274 = CARTESIAN_POINT ( 'NONE',  ( 52.57664461997821093, 53.40051614449765793, 8.007379884777206414 ) ) ;
#2276 = ADVANCED_FACE ( 'NONE', ( #3358 ), #1137, .F. ) ;
#2275 = ORIENTED_EDGE ( 'NONE', *, *, #12482, .F. ) ;
#2277 = ORIENTED_EDGE ( 'NONE', *, *, #2467, .T. ) ;
#2278 = VERTEX_POINT ( 'NONE', #6551 ) ;
#2279 = ORIENTED_EDGE ( 'NONE', *, *, #2720, .T. ) ;
#2280 = LINE ( 'NONE', #8661, #12207 ) ;
#2281 = FACE_OUTER_BOUND ( 'NONE', #3955, .T. ) ;
#2282 = ADVANCED_FACE ( 'NONE', ( #10880 ), #1395, .F. ) ;
#2284 = CIRCLE ( 'NONE', #10239, 5.000000000000007994 ) ;
#2283 = CARTESIAN_POINT ( 'NONE',  ( 3.973110223765528026, -0.6902454861566464928, 3.565797985667392034 ) ) ;
#2285 = DIRECTION ( 'NONE',  ( 0.000000000000000000, 0.000000000000000000, 1.000000000000000000 ) ) ;
#2286 = DIRECTION ( 'NONE',  ( -1.000000000000000000, 0.000000000000000000, 0.000000000000000000 ) ) ;
#2287 = CARTESIAN_POINT ( 'NONE',  ( 44.88205777487398507, 47.19948385550240744, -3.688883143319540814 ) ) ;
#2288 = CYLINDRICAL_SURFACE ( 'NONE', #11511, 4.000000000000003553 ) ;
#2289 = B_SPLINE_CURVE_WITH_KNOTS ( 'NONE', 3,
 ( #7864, #4816, #8280, #7245, #13299, #13506, #6147, #6002, #9312, #785, #10411, #9176, #6221, #10128, #712, #5033 ),
 .UNSPECIFIED., .F., .F.,
 ( 4, 3, 3, 3, 3, 4 ),
 ( 0.000000000000000000, 5.303647860849932744E-05, 0.0001057093501027352823, 0.0001642058037231763413, 0.0002210073443958810151, 0.0002236769549542870245 ),
 .UNSPECIFIED. ) ;
#2290 = EDGE_CURVE ( 'NONE', #6976, #8572, #4455, .T. ) ;
#2291 = CARTESIAN_POINT ( 'NONE',  ( 45.86712807150329496, 63.70051614449766220, 5.649768623646139964 ) ) ;
#2292 = B_SPLINE_CURVE_WITH_KNOTS ( 'NONE', 3,
 ( #8665, #286, #3405, #4509, #4371, #11976 ),
 .UNSPECIFIED., .F., .F.,
 ( 4, 2, 4 ),
 ( 0.002365888236227967761, 0.003551327329835077609, 0.004736766423442186590 ),
 .UNSPECIFIED. ) ;
#2293 = EDGE_CURVE ( 'NONE', #11760, #5079, #4909, .T. ) ;
#2294 = CARTESIAN_POINT ( 'NONE',  ( -31.74999999999995737, 0.000000000000000000, 0.000000000000000000 ) ) ;
#2295 = DIRECTION ( 'NONE',  ( 0.000000000000000000, 0.000000000000000000, -1.000000000000000000 ) ) ;
#2296 = CARTESIAN_POINT ( 'NONE',  ( 42.63976443033212860, 58.00051614449765225, -0.02388180880514948964 ) ) ;
#2297 = CARTESIAN_POINT ( 'NONE',  ( 44.88205777487398507, 61.19948385550241454, -3.688883143319540814 ) ) ;
#2298 = VECTOR ( 'NONE', #9222, 1000.000000000000000 ) ;
#2299 = ORIENTED_EDGE ( 'NONE', *, *, #6921, .T. ) ;
#2300 = ADVANCED_FACE ( 'NONE', ( #11997 ), #12882, .T. ) ;
#2301 = LINE ( 'NONE', #4320, #4399 ) ;
#2302 = VECTOR ( 'NONE', #6827, 1000.000000000000000 ) ;
#2303 = ORIENTED_EDGE ( 'NONE', *, *, #7828, .T. ) ;
#2304 = CARTESIAN_POINT ( 'NONE',  ( -74.99999999999998579, -2.602085213965210642E-14, 0.000000000000000000 ) ) ;
#2305 = DIRECTION ( 'NONE',  ( -0.9697813467099857254, -0.2439756946365076173, 1.379242460255691792E-22 ) ) ;
#2306 = CARTESIAN_POINT ( 'NONE',  ( 2.449293598294706513E-15, -20.00000000000000000, -9.000000000000000000 ) ) ;
#2307 = FILL_AREA_STYLE_COLOUR ( '', #4417 ) ;
#2308 = CARTESIAN_POINT ( 'NONE',  ( 56.66441430157296821, 48.09948385550240602, 2.141517661632100111 ) ) ;
#2309 = VECTOR ( 'NONE', #4488, 1000.000000000000000 ) ;
#2310 = DIRECTION ( 'NONE',  ( -1.000000000000000000, -0.000000000000000000, -0.000000000000000000 ) ) ;
#2311 = CARTESIAN_POINT ( 'NONE',  ( 44.28664221472221385, 49.90051614449766504, 1.832500667257213722 ) ) ;
#2312 = DIRECTION ( 'NONE',  ( -0.000000000000000000, -0.000000000000000000, 1.000000000000000000 ) ) ;
#2313 = DIRECTION ( 'NONE',  ( 0.000000000000000000, 1.000000000000000000, 0.000000000000000000 ) ) ;
#2314 = FILL_AREA_STYLE_COLOUR ( '', #9465 ) ;
#2315 = CARTESIAN_POINT ( 'NONE',  ( 55.94051828345050836, 61.79948385550239465, -4.345558710429104465 ) ) ;
#2316 = CARTESIAN_POINT ( 'NONE',  ( -74.99999999999997158, -39.99999999999998579, 10.00000000000000000 ) ) ;
#2317 = ORIENTED_EDGE ( 'NONE', *, *, #5140, .F. ) ;
#2318 = PRODUCT_DEFINITION_CONTEXT ( 'detailed design', #440, 'design' ) ;
#2319 = VERTEX_POINT ( 'NONE', #241 ) ;
#2320 = ORIENTED_EDGE ( 'NONE', *, *, #8072, .F. ) ;
#2321 = CARTESIAN_POINT ( 'NONE',  ( 4.114405500665256454, 4.051151509359430136, -5.737475420082528345E-17 ) ) ;
#2322 = CARTESIAN_POINT ( 'NONE',  ( 1.391697335622810172, 4.043246145443375461, -3.503898532754365913 ) ) ;
#2323 = CARTESIAN_POINT ( 'NONE',  ( 4.158806965674310518, -4.075748668183988066, -0.05940377217583901054 ) ) ;
#2324 = CARTESIAN_POINT ( 'NONE',  ( -22.00000000000000000, -19.99999999999999289, -20.00000000000000000 ) ) ;
#2325 = CARTESIAN_POINT ( 'NONE',  ( 54.09612160359786515, 53.69948385550240744, -5.676469297603166098 ) ) ;
#2326 = CARTESIAN_POINT ( 'NONE',  ( 45.90387839640208512, 54.30051614449765651, -5.676469297603124353 ) ) ;
#2327 = EDGE_CURVE ( 'NONE', #9556, #2018, #7651, .T. ) ;
#2328 = DIRECTION ( 'NONE',  ( 0.000000000000000000, 0.000000000000000000, -1.000000000000000000 ) ) ;
#2329 = CARTESIAN_POINT ( 'NONE',  ( 56.65037692655918988, 51.89948385550241028, -2.184720259617163762 ) ) ;
#2330 = FILL_AREA_STYLE_COLOUR ( '', #3572 ) ;
#2331 = CARTESIAN_POINT ( 'NONE',  ( 47.37792948025162332, 59.39948385550240317, -7.992620115222770494 ) ) ;
#2332 = ORIENTED_EDGE ( 'NONE', *, *, #6924, .F. ) ;
#2333 = ORIENTED_EDGE ( 'NONE', *, *, #6132, .F. ) ;
#2334 = CARTESIAN_POINT ( 'NONE',  ( 62.50000000000000000, 32.50000000000001421, 15.00000000000000000 ) ) ;
#2335 = VECTOR ( 'NONE', #2798, 1000.000000000000000 ) ;
#2336 = LINE ( 'NONE', #5536, #3110 ) ;
#2337 = VECTOR ( 'NONE', #889, 1000.000000000000114 ) ;
#2338 = CARTESIAN_POINT ( 'NONE',  ( 55.11794222512599362, 52.80051614449766362, -3.688883143319583446 ) ) ;
#2339 = CARTESIAN_POINT ( 'NONE',  ( 43.34962307344078880, 64.10051614449766078, -2.184720259617096705 ) ) ;
#2340 = CARTESIAN_POINT ( 'NONE',  ( 41.58830220609386430, 64.00051614449765225, -0.02388180880514929535 ) ) ;
#2341 = CARTESIAN_POINT ( 'NONE',  ( 47.70284917648453415, 57.39948385550241028, -6.992620115222774047 ) ) ;
#2342 = CARTESIAN_POINT ( 'NONE',  ( -12.99038105676659427, -12.50000000000003020, 9.000000000000000000 ) ) ;
#2343 = CARTESIAN_POINT ( 'NONE',  ( 56.79116909180259398, 55.20051614449766220, 4.963592699178938972 ) ) ;
#2344 = PRODUCT_DEFINITION_SHAPE ( 'NONE', 'NONE',  #13667 ) ;
#2346 = EDGE_CURVE ( 'NONE', #4780, #6905, #13357, .T. ) ;
#2345 = ORIENTED_EDGE ( 'NONE', *, *, #3394, .F. ) ;
#2347 = ORIENTED_EDGE ( 'NONE', *, *, #10264, .F. ) ;
#2348 = ORIENTED_EDGE ( 'NONE', *, *, #4024, .F. ) ;
#2349 = ORIENTED_EDGE ( 'NONE', *, *, #7292, .F. ) ;
#2350 = DIRECTION ( 'NONE',  ( -0.000000000000000000, -0.000000000000000000, 1.000000000000000000 ) ) ;
#2351 = LINE ( 'NONE', #5619, #6380 ) ;
#2352 = EDGE_CURVE ( 'NONE', #4274, #3871, #12836, .T. ) ;
#2353 = CARTESIAN_POINT ( 'NONE',  ( -74.99999999999997158, -7.499999999999971578, -20.00000000000000000 ) ) ;
#2354 = FACE_BOUND ( 'NONE', #4919, .T. ) ;
#2355 = CARTESIAN_POINT ( 'NONE',  ( 44.91013252490152752, 56.79948385550240175, 3.727524721679198461 ) ) ;
#2356 = CARTESIAN_POINT ( 'NONE',  ( 52.25172492374528588, 49.40051614449766504, 7.007379884777204637 ) ) ;
#2357 = CARTESIAN_POINT ( 'NONE',  ( 43.34962307344078880, 64.10051614449766078, -2.184720259617096705 ) ) ;
#2358 = DIRECTION ( 'NONE',  ( 0.000000000000000000, 0.000000000000000000, 1.000000000000000000 ) ) ;
#2359 = CARTESIAN_POINT ( 'NONE',  ( 0.1983443223721582938, 5.300482436767278038, 0.8192951148925896598 ) ) ;
#2360 = CARTESIAN_POINT ( 'NONE',  ( 54.09612160359792199, 57.30051614449765651, 5.676469297603124353 ) ) ;
#2361 = CARTESIAN_POINT ( 'NONE',  ( 53.54508667620428497, 62.29948385550241596, 4.840751629271157874 ) ) ;
#2362 = EDGE_CURVE ( 'NONE', #439, #6571, #10852, .T. ) ;
#2363 = ORIENTED_EDGE ( 'NONE', *, *, #3106, .T. ) ;
#2364 = DIRECTION ( 'NONE',  ( -0.000000000000000000, 0.000000000000000000, -1.000000000000000000 ) ) ;
#2365 = EDGE_CURVE ( 'NONE', #10456, #10143, #10950, .T. ) ;
#2366 = ORIENTED_EDGE ( 'NONE', *, *, #10588, .F. ) ;
#2367 = CARTESIAN_POINT ( 'NONE',  ( 6.196878017913834746, 1.924500897298752955, 5.000000000000000000 ) ) ;
#2368 = ADVANCED_BREP_SHAPE_REPRESENTATION ( '', ( #5429, #430 ), #11038 ) ;
#2369 = EDGE_CURVE ( 'NONE', #3263, #2448, #1437, .T. ) ;
#2370 = CARTESIAN_POINT ( 'NONE',  ( -30.00000000000000000, -7.500000000000005329, -10.00000000000000711 ) ) ;
#2371 = DIRECTION ( 'NONE',  ( 0.000000000000000000, 0.000000000000000000, -1.000000000000000000 ) ) ;
#2372 = CARTESIAN_POINT ( 'NONE',  ( 56.65037692655918988, 47.89948385550240317, -2.184720259617163762 ) ) ;
#2373 =( GEOMETRIC_REPRESENTATION_CONTEXT ( 3 ) GLOBAL_UNCERTAINTY_ASSIGNED_CONTEXT ( ( #8960 ) ) GLOBAL_UNIT_ASSIGNED_CONTEXT ( ( #2560, #9691, #5550 ) ) REPRESENTATION_CONTEXT ( 'NONE', 'WORKASPACE' ) );
#2374 = CARTESIAN_POINT ( 'NONE',  ( -1.250000000000000000, -6.429618962271402616, -1.000000000000000000 ) ) ;
#2375 = CARTESIAN_POINT ( 'NONE',  ( 48.02776887271750184, 57.60051614449765367, 5.992620115222795363 ) ) ;
#2376 = DIRECTION ( 'NONE',  ( -1.000000000000000000, -0.000000000000000000, -0.000000000000000000 ) ) ;
#2377 = PLANE ( 'NONE',  #11010 ) ;
#2378 = CARTESIAN_POINT ( 'NONE',  ( 0.000000000000000000, 0.000000000000000000, 5.000000000000000000 ) ) ;
#2379 = CARTESIAN_POINT ( 'NONE',  ( 56.30877334542961421, 47.99948385550239038, -0.02388180880520959434 ) ) ;
#2380 = CARTESIAN_POINT ( 'NONE',  ( 3.309651814758564736, -5.455921364805393026, -1.000000000000000000 ) ) ;
#2381 = ORIENTED_EDGE ( 'NONE', *, *, #4240, .T. ) ;
#2382 =( REPRESENTATION_RELATIONSHIP ('NONE','NONE', #5328, #10521 ) REPRESENTATION_RELATIONSHIP_WITH_TRANSFORMATION ( #13256 )SHAPE_REPRESENTATION_RELATIONSHIP( ) );
#2383 = AXIS2_PLACEMENT_3D ( 'NONE', #1612, #6755, #5721 ) ;
#2384 = VERTEX_POINT ( 'NONE', #561 ) ;
#2385 = DIRECTION ( 'NONE',  ( 1.000000000000000000, 0.000000000000000000, 0.000000000000000000 ) ) ;
#2386 = CARTESIAN_POINT ( 'NONE',  ( 2.804994570502171047, 3.229033611042449792, -3.526374918436834704 ) ) ;
#2387 = CARTESIAN_POINT ( 'NONE',  ( 0.4465819873852002742, 2.886751345948125547, 4.999999999999999112 ) ) ;
#2388 = CARTESIAN_POINT ( 'NONE',  ( -62.49999999999997158, 32.50000000000001421, 15.00000000000000000 ) ) ;
#2389 = CARTESIAN_POINT ( 'NONE',  ( 13.67449106481174148, -26.16508670809939829, -9.000000000000000000 ) ) ;
#2390 = CARTESIAN_POINT ( 'NONE',  ( 44.03140696652193498, 51.19948385550240033, -4.306917132069424170 ) ) ;
#2391 = CARTESIAN_POINT ( 'NONE',  ( 42.63976443033212860, 52.00051614449766646, -0.02388180880514948964 ) ) ;
#2392 = AXIS2_PLACEMENT_3D ( 'NONE', #10166, #11198, #1719 ) ;
#2393 = LINE ( 'NONE', #12768, #11694 ) ;
#2394 = CARTESIAN_POINT ( 'NONE',  ( 44.05948171654949874, 52.79948385550240175, 4.345558710429105354 ) ) ;
#2395 = CIRCLE ( 'NONE', #9902, 8.105212085995399107 ) ;
#2396 = DIRECTION ( 'NONE',  ( 1.000000000000000000, 0.000000000000000000, -0.000000000000000000 ) ) ;
#2397 = B_SPLINE_CURVE_WITH_KNOTS ( 'NONE', 3,
 ( #3370, #7595, #4473, #6560, #1339, #2251, #6365, #9797 ),
 .UNSPECIFIED., .F., .F.,
 ( 4, 2, 2, 4 ),
 ( 0.002921158011986727237, 0.003648658599403079624, 0.004376159186819432445, 0.005831160361652135485 ),
 .UNSPECIFIED. ) ;
#2398 = CARTESIAN_POINT ( 'NONE',  ( 43.20883090819745576, 64.79948385550240175, 4.963592699179006473 ) ) ;
#2399 = ORIENTED_EDGE ( 'NONE', *, *, #9923, .F. ) ;
#2400 = ORIENTED_EDGE ( 'NONE', *, *, #13346, .F. ) ;
#2401 = ADVANCED_FACE ( 'NONE', ( #2725 ), #7917, .F. ) ;
#2402 = ORIENTED_EDGE ( 'NONE', *, *, #8307, .T. ) ;
#2403 = AXIS2_PLACEMENT_3D ( 'NONE', #9410, #3184, #12582 ) ;
#2404 = CARTESIAN_POINT ( 'NONE',  ( -75.00000000000001421, -2.602085213965211904E-14, 0.000000000000000000 ) ) ;
#2405 = DIRECTION ( 'NONE',  ( 0.000000000000000000, 0.000000000000000000, 1.000000000000000000 ) ) ;
#2406 = CARTESIAN_POINT ( 'NONE',  ( 44.88205777487401349, 55.80051614449766362, 3.688883143319584779 ) ) ;
#2407 = CARTESIAN_POINT ( 'NONE',  ( 45.90387839640208512, 64.30051614449766362, -5.676469297603124353 ) ) ;
#2408 = CARTESIAN_POINT ( 'NONE',  ( 42.38452918213188525, 55.09948385550241312, -2.450534656007040013 ) ) ;
#2409 = VECTOR ( 'NONE', #4142, 1000.000000000000000 ) ;
#2410 = CARTESIAN_POINT ( 'NONE',  ( 56.65037692655918988, 59.89948385550241028, -2.184720259617163762 ) ) ;
#2411 = CARTESIAN_POINT ( 'NONE',  ( 0.000000000000000000, 0.000000000000000000, 0.000000000000000000 ) ) ;
#2412 = CARTESIAN_POINT ( 'NONE',  ( 42.39856655714566358, 46.89948385550240317, 2.493737253992119207 ) ) ;
#2413 = AXIS2_PLACEMENT_3D ( 'NONE', #13508, #7430, #10344 ) ;
#2414 = VERTEX_POINT ( 'NONE', #3763 ) ;
#2415 = ORIENTED_EDGE ( 'NONE', *, *, #1328, .F. ) ;
#2416 = ORIENTED_EDGE ( 'NONE', *, *, #3382, .T. ) ;
#2417 = ORIENTED_EDGE ( 'NONE', *, *, #9417, .T. ) ;
#2418 = DIRECTION ( 'NONE',  ( 0.000000000000000000, 0.000000000000000000, 1.000000000000000000 ) ) ;
#2420 = VECTOR ( 'NONE', #2954, 1000.000000000000000 ) ;
#2419 = DIRECTION ( 'NONE',  ( -0.7071067811865530128, 8.659560562354868763E-17, -0.7071067811865421326 ) ) ;
#2421 = PRESENTATION_STYLE_ASSIGNMENT (( #3402 ) ) ;
#2422 = DIRECTION ( 'NONE',  ( -1.000000000000000000, -0.000000000000000000, -0.000000000000000000 ) ) ;
#2423 = FACE_OUTER_BOUND ( 'NONE', #4572, .T. ) ;
#2424 = CARTESIAN_POINT ( 'NONE',  ( 44.91013252490152752, 58.79948385550240175, 3.727524721679198461 ) ) ;
#2425 = CARTESIAN_POINT ( 'NONE',  ( 42.63976443033212149, 50.00051614449765935, -0.02388180880514948964 ) ) ;
#2426 = CARTESIAN_POINT ( 'NONE',  ( 42.39856655714564226, 52.10051614449766788, -2.493737253992044156 ) ) ;
#2427 = EDGE_CURVE ( 'NONE', #5888, #11823, #1669, .T. ) ;
#2428 = CARTESIAN_POINT ( 'NONE',  ( 2.449293598294706513E-15, -20.00000000000000000, 9.000000000000000000 ) ) ;
#2429 = CARTESIAN_POINT ( 'NONE',  ( 2.000000000000000000, 1.773042676681340524, -2.059984127722458425E-15 ) ) ;
#2430 = CARTESIAN_POINT ( 'NONE',  ( 47.70284917648459100, 63.60051614449766078, 6.992620115222796251 ) ) ;
#2431 =( GEOMETRIC_REPRESENTATION_CONTEXT ( 3 ) GLOBAL_UNCERTAINTY_ASSIGNED_CONTEXT ( ( #3299 ) ) GLOBAL_UNIT_ASSIGNED_CONTEXT ( ( #3506, #4545, #13541 ) ) REPRESENTATION_CONTEXT ( 'NONE', 'WORKASPACE' ) );
#2432 = AXIS2_PLACEMENT_3D ( 'NONE', #6382, #10446, #3255 ) ;
#2433 = EDGE_CURVE ( 'NONE', #579, #12390, #11836, .T. ) ;
#2434 = VERTEX_POINT ( 'NONE', #11156 ) ;
#2435 = CARTESIAN_POINT ( 'NONE',  ( 0.000000000000000000, 0.000000000000000000, -1.000000000000000000 ) ) ;
#2436 = VERTEX_POINT ( 'NONE', #3900 ) ;
#2437 = DIRECTION ( 'NONE',  ( -0.000000000000000000, -0.000000000000000000, -1.000000000000000000 ) ) ;
#2438 = DIRECTION ( 'NONE',  ( 1.000000000000000000, 0.000000000000000000, 0.000000000000000000 ) ) ;
#2439 = CARTESIAN_POINT ( 'NONE',  ( 4.050536630291690976, 3.778525289263159781, 0.5912575323401418892 ) ) ;
#2440 = CARTESIAN_POINT ( 'NONE',  ( 56.66441430157296821, 60.09948385550240602, 2.141517661632100111 ) ) ;
#2441 = FACE_OUTER_BOUND ( 'NONE', #1002, .T. ) ;
#2442 = CARTESIAN_POINT ( 'NONE',  ( 49.97728705011494554, 55.50051614449766646, 6.000000000000000888 ) ) ;
#2443 = DIRECTION ( 'NONE',  ( -0.000000000000000000, -0.000000000000000000, -1.000000000000000000 ) ) ;
#2444 = DIRECTION ( 'NONE',  ( 0.4999999999999977796, 0.8660254037844398178, 0.000000000000000000 ) ) ;
#2445 = DIRECTION ( 'NONE',  ( -1.000000000000000000, -0.000000000000000000, -0.000000000000000000 ) ) ;
#2446 = CARTESIAN_POINT ( 'NONE',  ( 57.36023556966787851, 63.99948385550241881, -0.02388180880522424582 ) ) ;
#2447 = CYLINDRICAL_SURFACE ( 'NONE', #13079, 12.49999999999999645 ) ;
#2448 = VERTEX_POINT ( 'NONE', #5712 ) ;
#2449 = ORIENTED_EDGE ( 'NONE', *, *, #4923, .T. ) ;
#2450 = AXIS2_PLACEMENT_3D ( 'NONE', #4261, #6543, #11529 ) ;
#2451 = ADVANCED_FACE ( 'NONE', ( #1674 ), #10115, .T. ) ;
#2452 = ORIENTED_EDGE ( 'NONE', *, *, #7450, .F. ) ;
#2453 = DIRECTION ( 'NONE',  ( -1.000000000000000000, -0.000000000000000000, -0.000000000000000000 ) ) ;
#2454 = CARTESIAN_POINT ( 'NONE',  ( -0.02448733951239248641, -4.877042772274742255, -3.751161874094027571 ) ) ;
#2455 = FACE_OUTER_BOUND ( 'NONE', #12631, .T. ) ;
#2456 = CARTESIAN_POINT ( 'NONE',  ( 6.362374563307939823, 3.415000007733389076, 4.302769906042884784 ) ) ;
#2457 = CARTESIAN_POINT ( 'NONE',  ( -62.49999999999997158, 32.50000000000001421, 15.00000000000000000 ) ) ;
#2458 = CARTESIAN_POINT ( 'NONE',  ( 44.05948171654949874, 54.79948385550240886, 4.345558710429104465 ) ) ;
#2459 = CIRCLE ( 'NONE', #11291, 2.649999999999985700 ) ;
#2460 = CARTESIAN_POINT ( 'NONE',  ( 55.94051828345053679, 51.20051614449766220, 4.345558710429044069 ) ) ;
#2461 = DIRECTION ( 'NONE',  ( -0.000000000000000000, -0.000000000000000000, -1.000000000000000000 ) ) ;
#2462 = VECTOR ( 'NONE', #680, 1000.000000000000227 ) ;
#2463 = CIRCLE ( 'NONE', #3137, 2.149999999999999023 ) ;
#2464 = CARTESIAN_POINT ( 'NONE',  ( 56.65037692655918988, 53.89948385550240317, -2.184720259617163762 ) ) ;
#2465 = EDGE_CURVE ( 'NONE', #13025, #2854, #1225, .T. ) ;
#2466 = CARTESIAN_POINT ( 'NONE',  ( 49.97728705011488159, 45.49948385550240459, -7.000000000000000888 ) ) ;
#2467 = EDGE_CURVE ( 'NONE', #8373, #1065, #8973, .T. ) ;
#2468 = CARTESIAN_POINT ( 'NONE',  ( 52.57664461997811856, 63.59948385550239891, -8.007379884777229506 ) ) ;
#2469 = ORIENTED_EDGE ( 'NONE', *, *, #6056, .T. ) ;
#2470 = VERTEX_POINT ( 'NONE', #9090 ) ;
#2471 = DIRECTION ( 'NONE',  ( 0.8571673013836855759, 1.049727191973305147E-16, -0.5150380737757258576 ) ) ;
#2472 = AXIS2_PLACEMENT_3D ( 'NONE', #8031, #13399, #11132 ) ;
#2473 = EDGE_LOOP ( 'NONE', ( #8167, #11481, #1970, #29 ) ) ;
#2474 = CARTESIAN_POINT ( 'NONE',  ( 18.00000000000000355, -20.00000000000000000, -20.00000000000000000 ) ) ;
#2475 = VECTOR ( 'NONE', #468, 1000.000000000000000 ) ;
#2476 = DIRECTION ( 'NONE',  ( 0.000000000000000000, 0.000000000000000000, -1.000000000000000000 ) ) ;
#2477 =( BOUNDED_SURFACE ( )  B_SPLINE_SURFACE ( 3, 2, ( 
 ( #11622, #7349, #5212 ),
 ( #2136, #10511, #4154 ),
 ( #2007, #5273, #4290 ),
 ( #11561, #5408, #4093 ),
 ( #69, #8378, #2201 ),
 ( #13543, #8314, #6445 ) ),
 .UNSPECIFIED., .F., .F., .T. ) 
 B_SPLINE_SURFACE_WITH_KNOTS ( ( 4, 2, 4 ),
 ( 3, 3 ),
 ( 0.02367865728600888897, 0.02663179453327094853, 0.02958493178053300809 ),
 ( 0.000000000000000000, 1.000000000000000000 ),
 .UNSPECIFIED. ) 
 GEOMETRIC_REPRESENTATION_ITEM ( )  RATIONAL_B_SPLINE_SURFACE ( (
 ( 1.000000000000000000, 0.8047781103519399126, 1.000000000000000000),
 ( 1.000000000000000000, 0.8123785825980039954, 1.000000000000000000),
 ( 1.000000000000000000, 0.8190671539288042480, 1.000000000000000000),
 ( 1.000000000000000000, 0.8192352255335092481, 1.000000000000000000),
 ( 1.000000000000000000, 0.8126129676835893711, 1.000000000000000000),
 ( 1.000000000000000000, 0.8047712537969730073, 1.000000000000000000) ) ) 
 REPRESENTATION_ITEM ( '' )  SURFACE ( )  );
#2478 = CARTESIAN_POINT ( 'NONE',  ( 48.07319477248762496, 56.40051614449765793, -6.007379884777208190 ) ) ;
#2479 = CARTESIAN_POINT ( 'NONE',  ( 42.63976443033212149, 64.00051614449765225, -0.02388180880514948964 ) ) ;
#2480 = CARTESIAN_POINT ( 'NONE',  ( 45.31609314410967926, 54.69948385550240033, 6.485486291978119766 ) ) ;
#2481 = EDGE_CURVE ( 'NONE', #1895, #898, #1276, .T. ) ;
#2482 = CARTESIAN_POINT ( 'NONE',  ( 57.36023556966787851, 57.99948385550239038, -0.02388180880522424582 ) ) ;
#2483 = CARTESIAN_POINT ( 'NONE',  ( 50.00000000000000000, 15.00000000000000000, 4.000000000000003553 ) ) ;
#2484 = CARTESIAN_POINT ( 'NONE',  ( 52.57664461997821093, 63.40051614449765083, 8.007379884777206414 ) ) ;
#2485 = AXIS2_PLACEMENT_3D ( 'NONE', #12752, #6985, #10884 ) ;
#2486 = VERTEX_POINT ( 'NONE', #13086 ) ;
#2487 = ITEM_DEFINED_TRANSFORMATION ( 'NONE', 'NONE', #8615,  #430 ) ;
#2488 = ORIENTED_EDGE ( 'NONE', *, *, #8643, .T. ) ;
#2489 = EDGE_LOOP ( 'NONE', ( #2927, #10019, #8133, #3347, #10384, #2230, #11123 ) ) ;
#2490 = VERTEX_POINT ( 'NONE', #7853 ) ;
#2491 = CARTESIAN_POINT ( 'NONE',  ( -2.344047193898593395, -3.265465875126480455, -1.054683074273691752E-14 ) ) ;
#2492 = CLOSED_SHELL ( 'NONE', ( #10075, #3181, #810, #918, #7463, #6548, #11141, #3731, #9467, #10389, #12183, #13131, #5361, #8892, #9764, #3910, #752, #9684, #1131, #1872, #8900, #7361 ) ) ;
#2493 = FACE_OUTER_BOUND ( 'NONE', #8185, .T. ) ;
#2494 =( LENGTH_UNIT ( ) NAMED_UNIT ( * ) SI_UNIT ( .MILLI., .METRE. ) );
#2495 = CARTESIAN_POINT ( 'NONE',  ( -0.1481481481481481122, -4.797713218419819903, -1.000000000000000000 ) ) ;
#2496 = DIRECTION ( 'NONE',  ( -1.000000000000000000, -0.000000000000000000, -0.000000000000000000 ) ) ;
#2497 = CARTESIAN_POINT ( 'NONE',  ( 55.69932041026404335, 57.89948385550241028, -1.875703265242203432 ) ) ;
#2498 = CARTESIAN_POINT ( 'NONE',  ( 44.05948171654945611, 50.20051614449765509, -4.345558710429044069 ) ) ;
#2499 = CARTESIAN_POINT ( 'NONE',  ( 43.20883090819742023, 50.20051614449766220, -4.963592699178938972 ) ) ;
#2500 = DIRECTION ( 'NONE',  ( -1.734723475976807341E-16, -1.000000000000000000, 0.000000000000000000 ) ) ;
#2501 = CARTESIAN_POINT ( 'NONE',  ( 32.49999999999998579, 5.000000000000018652, 5.000000000000003553 ) ) ;
#2502 = CARTESIAN_POINT ( 'NONE',  ( 56.66441430157294690, 60.90051614449766504, -2.141517661632166281 ) ) ;
#2503 = ORIENTED_EDGE ( 'NONE', *, *, #12212, .F. ) ;
#2504 = CARTESIAN_POINT ( 'NONE',  ( -29.99999999999999645, 40.00000000000000000, 10.00000000000000000 ) ) ;
#2505 = VECTOR ( 'NONE', #8545, 1000.000000000000000 ) ;
#2506 = ORIENTED_EDGE ( 'NONE', *, *, #3585, .T. ) ;
#2507 = CARTESIAN_POINT ( 'NONE',  ( 0.4465819873849485311, -2.886751345948517677, -5.000000000000000000 ) ) ;
#2508 = CYLINDRICAL_SURFACE ( 'NONE', #2075, 2.396904916527700102 ) ;
#2509 = CYLINDRICAL_SURFACE ( 'NONE', #12395, 5.000000000000000000 ) ;
#2510 = APPLICATION_PROTOCOL_DEFINITION ( 'draft international standard', 'automotive_design', 1998, #4778 ) ;
#2511 = CARTESIAN_POINT ( 'NONE',  ( 50.02271294988512551, 58.49948385550241170, 7.000000000000000888 ) ) ;
#2512 = CARTESIAN_POINT ( 'NONE',  ( 44.28664221472221385, 59.90051614449767214, 1.832500667257213722 ) ) ;
#2513 = VECTOR ( 'NONE', #8590, 1000.000000000000000 ) ;
#2514 = DIRECTION ( 'NONE',  ( 1.000000000000000000, 0.000000000000000000, 0.000000000000000000 ) ) ;
#2515 = DIRECTION ( 'NONE',  ( 0.000000000000000000, 0.000000000000000000, -1.000000000000000000 ) ) ;
#2516 = CARTESIAN_POINT ( 'NONE',  ( 48.02776887271750184, 61.60051614449765367, 5.992620115222795363 ) ) ;
#2517 = CARTESIAN_POINT ( 'NONE',  ( 55.71335778527780747, 48.09948385550240602, 1.832500667257165983 ) ) ;
#2518 = CARTESIAN_POINT ( 'NONE',  ( -31.74999999999995737, 2.449293598294707893E-16, -2.000000000000000888 ) ) ;
#2519 = ORIENTED_EDGE ( 'NONE', *, *, #777, .F. ) ;
#2520 = VECTOR ( 'NONE', #502, 1000.000000000000000 ) ;
#2521 = AXIS2_PLACEMENT_3D ( 'NONE', #1007, #9459, #8431 ) ;
#2522 = ORIENTED_EDGE ( 'NONE', *, *, #11531, .F. ) ;
#2523 = PLANE ( 'NONE',  #2611 ) ;
#2524 = CIRCLE ( 'NONE', #6949, 12.49999999999999645 ) ;
#2525 = CARTESIAN_POINT ( 'NONE',  ( 4.204015924366189871, -1.626724848190933548, -3.610627190413393084 ) ) ;
#2526 = CARTESIAN_POINT ( 'NONE',  ( 5.000000000000003553, -20.00000000000000000, -9.999999999999994671 ) ) ;
#2527 = LINE ( 'NONE', #10962, #246 ) ;
#2528 = DIRECTION ( 'NONE',  ( -1.000000000000000000, 0.000000000000000000, 0.000000000000000000 ) ) ;
#2529 = EDGE_CURVE ( 'NONE', #4887, #5545, #12500, .T. ) ;
#2530 = CARTESIAN_POINT ( 'NONE',  ( 45.86712807150329496, 55.70051614449766220, 5.649768623646139964 ) ) ;
#2531 = CARTESIAN_POINT ( 'NONE',  ( 2.000000000000000000, 0.000000000000000000, 0.000000000000000000 ) ) ;
#2532 = CARTESIAN_POINT ( 'NONE',  ( 44.03140696652192787, 49.19948385550240033, -4.306917132069425058 ) ) ;
#2533 = CARTESIAN_POINT ( 'NONE',  ( 43.34962307344081012, 46.89948385550240317, 2.184720259617164650 ) ) ;
#2534 = CONICAL_SURFACE ( 'NONE', #13343, 4.000000000000000000, 0.8911886515913786111 ) ;
#2535 = CARTESIAN_POINT ( 'NONE',  ( 52.62207051974839089, 60.39948385550241028, 7.992620115222770494 ) ) ;
#2536 = EDGE_CURVE ( 'NONE', #12922, #5946, #12064, .T. ) ;
#2537 = ORIENTED_EDGE ( 'NONE', *, *, #11577, .F. ) ;
#2538 = EDGE_LOOP ( 'NONE', ( #4728, #1208, #10269, #10720 ) ) ;
#2539 = CARTESIAN_POINT ( 'NONE',  ( 3.948111298835276894, -0.6968132764964354298, -3.500000000000154987 ) ) ;
#2540 = EDGE_CURVE ( 'NONE', #10855, #3640, #5783, .T. ) ;
#2541 = ORIENTED_EDGE ( 'NONE', *, *, #2369, .T. ) ;
#2542 = EDGE_CURVE ( 'NONE', #9150, #5892, #555, .T. ) ;
#2543 = DIRECTION ( 'NONE',  ( 0.000000000000000000, 0.000000000000000000, -1.000000000000000000 ) ) ;
#2544 = EDGE_CURVE ( 'NONE', #614, #408, #1602, .T. ) ;
#2545 = DIRECTION ( 'NONE',  ( -1.000000000000000000, 0.000000000000000000, 0.000000000000000000 ) ) ;
#2546 = CARTESIAN_POINT ( 'NONE',  ( 50.02271294988506156, 54.50051614449765935, -6.000000000000000888 ) ) ;
#2547 = PRODUCT_DEFINITION_SHAPE ( 'NONE', 'NONE',  #12316 ) ;
#2548 = FACE_OUTER_BOUND ( 'NONE', #2785, .T. ) ;
#2549 = CARTESIAN_POINT ( 'NONE',  ( 54.72065718078924590, 52.29948385550240886, 6.458785618021043895 ) ) ;
#2550 = CARTESIAN_POINT ( 'NONE',  ( 45.90387839640214196, 54.69948385550240744, 5.676469297603166098 ) ) ;
#2551 = CARTESIAN_POINT ( 'NONE',  ( 1.925929944387235853E-31, 15.00000000000001599, 15.00000000000000000 ) ) ;
#2552 = CARTESIAN_POINT ( 'NONE',  ( 50.02271294988505446, 64.50051614449766646, -8.000000000000001776 ) ) ;
#2553 = ORIENTED_EDGE ( 'NONE', *, *, #10454, .T. ) ;
#2554 = ORIENTED_EDGE ( 'NONE', *, *, #3984, .T. ) ;
#2555 = AXIS2_PLACEMENT_3D ( 'NONE', #1960, #6203, #12733 ) ;
#2556 = ORIENTED_EDGE ( 'NONE', *, *, #4759, .F. ) ;
#2557 = ORIENTED_EDGE ( 'NONE', *, *, #8401, .F. ) ;
#2558 = AXIS2_PLACEMENT_3D ( 'NONE', #11443, #11646, #9376 ) ;
#2559 = CARTESIAN_POINT ( 'NONE',  ( 6.371506350351443970, 3.439339428956429856, -4.260454149911179655 ) ) ;
#2560 =( LENGTH_UNIT ( ) NAMED_UNIT ( * ) SI_UNIT ( .MILLI., .METRE. ) );
#2561 = EDGE_CURVE ( 'NONE', #9809, #2590, #12608, .T. ) ;
#2562 = SURFACE_SIDE_STYLE ('',( #8865 ) ) ;
#2563 = CYLINDRICAL_SURFACE ( 'NONE', #6455, 1.500000000000001332 ) ;
#2564 = DIRECTION ( 'NONE',  ( -0.000000000000000000, -0.000000000000000000, 1.000000000000000000 ) ) ;
#2565 = CARTESIAN_POINT ( 'NONE',  ( 53.50833635130540955, 57.69948385550241454, -4.867452303228209765 ) ) ;
#2566 = CARTESIAN_POINT ( 'NONE',  ( 50.02271294988505446, 46.50051614449765935, -7.000000000000000888 ) ) ;
#2567 = CARTESIAN_POINT ( 'NONE',  ( 41.58830220609386430, 52.00051614449766646, -0.02388180880514929535 ) ) ;
#2568 =( REPRESENTATION_RELATIONSHIP ('NONE','NONE', #5328, #180 ) REPRESENTATION_RELATIONSHIP_WITH_TRANSFORMATION ( #13188 )SHAPE_REPRESENTATION_RELATIONSHIP( ) );
#2569 = CARTESIAN_POINT ( 'NONE',  ( 20.00000000000000000, -14.99999999999999289, -23.00000000000000000 ) ) ;
#2570 = CARTESIAN_POINT ( 'NONE',  ( 54.08601618280673051, 45.00000000000005684, -5.120135501906166731 ) ) ;
#2571 = COLOUR_RGB ( '',1.000000000000000000, 0.9490196078431372140, 0.9098039215686274384 ) ;
#2572 = CARTESIAN_POINT ( 'NONE',  ( 45.31609314410960820, 46.30051614449766362, -6.485486291978072693 ) ) ;
#2573 = ORIENTED_EDGE ( 'NONE', *, *, #6544, .T. ) ;
#2574 = CARTESIAN_POINT ( 'NONE',  ( 20.00000000000000000, -20.00000000000000000, -20.00000000000000000 ) ) ;
#2575 = ORIENTED_EDGE ( 'NONE', *, *, #1863, .T. ) ;
#2576 = EDGE_CURVE ( 'NONE', #12550, #2490, #4337, .T. ) ;
#2577 = EDGE_CURVE ( 'NONE', #7202, #5253, #10068, .T. ) ;
#2578 = CARTESIAN_POINT ( 'NONE',  ( 1.267864665251833278E-11, -20.00000000000000000, 9.000000000000000000 ) ) ;
#2579 = CARTESIAN_POINT ( 'NONE',  ( 3.950241966888156320, -2.668221755853644073, -2.378504353000863158 ) ) ;
#2580 = DIRECTION ( 'NONE',  ( 6.123233995736766036E-17, 0.000000000000000000, 1.000000000000000000 ) ) ;
#2581 = CARTESIAN_POINT ( 'NONE',  ( 44.05948171654949874, 54.79948385550241596, 4.345558710429105354 ) ) ;
#2582 = CARTESIAN_POINT ( 'NONE',  ( 56.30877334542961421, 61.00051614449765935, 0.02388180880515774693 ) ) ;
#2583 = DIRECTION ( 'NONE',  ( -0.7779254092217071648, -0.6283566325640553840, 0.000000000000000000 ) ) ;
#2584 = CARTESIAN_POINT ( 'NONE',  ( 6.270568613849413886, 4.911887854652841057, 1.704496029161937320 ) ) ;
#2585 = CARTESIAN_POINT ( 'NONE',  ( 55.08986747509849380, 63.20051614449766220, 3.727524721679155384 ) ) ;
#2586 = CARTESIAN_POINT ( 'NONE',  ( 44.91013252490152752, 48.79948385550240175, 3.727524721679198461 ) ) ;
#2587 = DIRECTION ( 'NONE',  ( -1.000000000000000000, -0.000000000000000000, -0.000000000000000000 ) ) ;
#2588 = VERTEX_POINT ( 'NONE', #3966 ) ;
#2589 = PRODUCT_DEFINITION_CONTEXT ( 'detailed design', #3366, 'design' ) ;
#2590 = VERTEX_POINT ( 'NONE', #4247 ) ;
#2591 = DIRECTION ( 'NONE',  ( -1.000000000000000000, 0.000000000000000000, 0.000000000000000000 ) ) ;
#2592 = DIRECTION ( 'NONE',  ( -1.000000000000000000, 0.000000000000000000, 0.000000000000000000 ) ) ;
#2593 = CARTESIAN_POINT ( 'NONE',  ( 0.000000000000000000, -3.031088913245534755, -1.750000000000001332 ) ) ;
#2594 =( NAMED_UNIT ( * ) PLANE_ANGLE_UNIT ( ) SI_UNIT ( $, .RADIAN. ) );
#2595 = DIRECTION ( 'NONE',  ( 1.000000000000000000, 3.469446951953615175E-16, 0.000000000000000000 ) ) ;
#2596 = DIRECTION ( 'NONE',  ( -1.000000000000000000, 0.000000000000000000, 0.000000000000000000 ) ) ;
#2597 = CARTESIAN_POINT ( 'NONE',  ( 55.96859303347802239, 58.80051614449764941, -4.306917132069484566 ) ) ;
#2598 = CARTESIAN_POINT ( 'NONE',  ( 6.357965579934049316, -1.995168835099641713, -5.108766517442258959 ) ) ;
#2599 = LINE ( 'NONE', #1552, #2302 ) ;
#2600 = ADVANCED_FACE ( 'NONE', ( #10261 ), #4179, .F. ) ;
#2601 = CARTESIAN_POINT ( 'NONE',  ( 52.25172492374522903, 49.59948385550240602, -7.007379884777225953 ) ) ;
#2602 = CARTESIAN_POINT ( 'NONE',  ( 52.29715082351547295, 48.39948385550240317, 6.992620115222774047 ) ) ;
#2603 = AXIS2_PLACEMENT_3D ( 'NONE', #8934, #600, #13263 ) ;
#2604 = CARTESIAN_POINT ( 'NONE',  ( 54.68390685589033495, 61.69948385550240744, -6.485486291978119766 ) ) ;
#2605 = ADVANCED_FACE ( 'NONE', ( #13493 ), #11296, .F. ) ;
#2606 = ORIENTED_EDGE ( 'NONE', *, *, #995, .T. ) ;
#2607 = ORIENTED_EDGE ( 'NONE', *, *, #6781, .F. ) ;
#2608 = CARTESIAN_POINT ( 'NONE',  ( 4.055487192203242941, 1.409979666030558354, -3.568038521265956664 ) ) ;
#2609 = ORIENTED_EDGE ( 'NONE', *, *, #5768, .F. ) ;
#2610 = DIRECTION ( 'NONE',  ( 1.000000000000000000, 0.000000000000000000, 0.000000000000000000 ) ) ;
#2611 = AXIS2_PLACEMENT_3D ( 'NONE', #4678, #13160, #9921 ) ;
#2612 = CARTESIAN_POINT ( 'NONE',  ( 6.367873360227558344, -2.886751345948133984, -5.000000000000000000 ) ) ;
#2613 = CARTESIAN_POINT ( 'NONE',  ( 49.97728705011494554, 51.50051614449765935, 6.000000000000000888 ) ) ;
#2614 = CYLINDRICAL_SURFACE ( 'NONE', #6233, 15.00000000000000000 ) ;
#2615 = CARTESIAN_POINT ( 'NONE',  ( 42.38452918213188525, 51.09948385550240602, -2.450534656007040013 ) ) ;
#2616 = CARTESIAN_POINT ( 'NONE',  ( 44.05948171654949874, 56.79948385550240886, 4.345558710429105354 ) ) ;
#2617 = CARTESIAN_POINT ( 'NONE',  ( -62.49999999999997158, 45.00000000000001421, 9.999999999999998224 ) ) ;
#2618 = CARTESIAN_POINT ( 'NONE',  ( 50.02271294988513972, 46.49948385550240459, 8.000000000000001776 ) ) ;
#2619 = AXIS2_PLACEMENT_3D ( 'NONE', #6603, #9844, #1321 ) ;
#2620 = ORIENTED_EDGE ( 'NONE', *, *, #5080, .T. ) ;
#2621 = ITEM_DEFINED_TRANSFORMATION ( 'NONE', 'NONE', #5529,  #430 ) ;
#2622 = AXIS2_PLACEMENT_3D ( 'NONE', #11016, #12266, #3968 ) ;
#2623 = ORIENTED_EDGE ( 'NONE', *, *, #1697, .T. ) ;
#2624 = ORIENTED_EDGE ( 'NONE', *, *, #6395, .T. ) ;
#2625 = ORIENTED_EDGE ( 'NONE', *, *, #9989, .F. ) ;
#2626 = VECTOR ( 'NONE', #10473, 1000.000000000000000 ) ;
#2627 = DIRECTION ( 'NONE',  ( -0.000000000000000000, -0.000000000000000000, -1.000000000000000000 ) ) ;
#2628 = FACE_OUTER_BOUND ( 'NONE', #13159, .T. ) ;
#2629 = COLOUR_RGB ( '',1.000000000000000000, 0.9490196078431372140, 0.9098039215686274384 ) ;
#2630 =( NAMED_UNIT ( * ) PLANE_ANGLE_UNIT ( ) SI_UNIT ( $, .RADIAN. ) );
#2631 = CIRCLE ( 'NONE', #11019, 1.500000000000000666 ) ;
#2632 = CARTESIAN_POINT ( 'NONE',  ( 51.97223112728254790, 58.39948385550241028, 5.992620115222778487 ) ) ;
#2633 = CARTESIAN_POINT ( 'NONE',  ( 49.97728705011495265, 45.50051614449765935, 7.000000000000000888 ) ) ;
#2634 = CARTESIAN_POINT ( 'NONE',  ( 54.72065718078918906, 50.70051614449766220, -6.458785618021089192 ) ) ;
#2635 = FILL_AREA_STYLE ('',( #3821 ) ) ;
#2636 = CARTESIAN_POINT ( 'NONE',  ( -62.49999999999997158, 32.50000000000001421, -9.999999999999998224 ) ) ;
#2637 = B_SPLINE_CURVE_WITH_KNOTS ( 'NONE', 3,
 ( #5166, #11372, #9434, #1891, #3072, #6136, #3006, #1961, #11437, #836 ),
 .UNSPECIFIED., .F., .F.,
 ( 4, 2, 2, 2, 4 ),
 ( 0.000000000000000000, 0.003112635120760290971, 0.004668952681140444913, 0.005447111461330522535, 0.006225270241520600156 ),
 .UNSPECIFIED. ) ;
#2638 = EDGE_CURVE ( 'NONE', #1386, #9920, #9498, .T. ) ;
#2639 = CARTESIAN_POINT ( 'NONE',  ( 43.33558569842706021, 61.90051614449766504, 2.141517661632167169 ) ) ;
#2640 = B_SPLINE_CURVE_WITH_KNOTS ( 'NONE', 3,
 ( #12607, #12732, #3140, #89, #7435 ),
 .UNSPECIFIED., .F., .F.,
 ( 4, 1, 4 ),
 ( 0.000000000000000000, 0.002309401076758505790, 0.004618802153517011580 ),
 .UNSPECIFIED. ) ;
#2641 = EDGE_CURVE ( 'NONE', #10476, #6120, #3235, .T. ) ;
#2642 = ORIENTED_EDGE ( 'NONE', *, *, #2257, .F. ) ;
#2643 = PRESENTATION_LAYER_ASSIGNMENT (  '', '', ( #5975 ) ) ;
#2644 = AXIS2_PLACEMENT_3D ( 'NONE', #6226, #2173, #8420 ) ;
#2645 = CARTESIAN_POINT ( 'NONE',  ( 1.411581201560190495E-15, 4.862606272033091592, -3.745885042887436622 ) ) ;
#2646 = EDGE_CURVE ( 'NONE', #5253, #4470, #13631, .T. ) ;
#2647 = ORIENTED_EDGE ( 'NONE', *, *, #1404, .T. ) ;
#2648 = DIRECTION ( 'NONE',  ( -4.082155997157844188E-16, 1.000000000000000000, 0.000000000000000000 ) ) ;
#2649 = CARTESIAN_POINT ( 'NONE',  ( 2.449293598294706513E-15, -20.00000000000000000, -9.000000000000000000 ) ) ;
#2650 = CARTESIAN_POINT ( 'NONE',  ( 43.33558569842703179, 57.09948385550240602, -2.141517661632099223 ) ) ;
#2651 = AXIS2_PLACEMENT_3D ( 'NONE', #3676, #6529, #10727 ) ;
#2652 = CARTESIAN_POINT ( 'NONE',  ( 53.54508667620424234, 58.70051614449765509, -4.840751629271188961 ) ) ;
#2653 = CARTESIAN_POINT ( 'NONE',  ( 3.973514160553462737, -2.741076955031366502, -2.383932505289870551 ) ) ;
#2654 = CARTESIAN_POINT ( 'NONE',  ( 0.000000000000000000, 0.5192545390863916310, -1.000000000000000000 ) ) ;
#2655 = CARTESIAN_POINT ( 'NONE',  ( 44.05948171654945611, 46.20051614449766930, -4.345558710429044069 ) ) ;
#2656 = CARTESIAN_POINT ( 'NONE',  ( 47.74827507625478518, 64.59948385550239891, 7.007379884777227730 ) ) ;
#2657 = CYLINDRICAL_SURFACE ( 'NONE', #12026, 12.49999999999999645 ) ;
#2658 = VERTEX_POINT ( 'NONE', #3141 ) ;
#2659 = ORIENTED_EDGE ( 'NONE', *, *, #2719, .T. ) ;
#2660 = VERTEX_POINT ( 'NONE', #11513 ) ;
#2661 = CARTESIAN_POINT ( 'NONE',  ( 8.673617379884035472E-16, 4.618802153517012954, -5.000000000000000000 ) ) ;
#2662 = CARTESIAN_POINT ( 'NONE',  ( 3.522875095019493141, -2.820352903225631369, -3.598441714920572299 ) ) ;
#2663 = B_SPLINE_CURVE_WITH_KNOTS ( 'NONE', 3,
 ( #2970, #6307, #7197, #11402, #1922, #6165, #5126, #8301 ),
 .UNSPECIFIED., .F., .F.,
 ( 4, 2, 2, 4 ),
 ( 0.005725059856848641743, 0.006314084072593626612, 0.006903108288338611481, 0.008081156719828581220 ),
 .UNSPECIFIED. ) ;
#2664 = LINE ( 'NONE', #12142, #9310 ) ;
#2665 = EDGE_CURVE ( 'NONE', #4232, #7288, #5165, .T. ) ;
#2666 = SURFACE_SIDE_STYLE ('',( #5658 ) ) ;
#2667 = CARTESIAN_POINT ( 'NONE',  ( 6.207530437345011087, 3.810448612249821565, 3.400109403952575882 ) ) ;
#2668 = DIRECTION ( 'NONE',  ( -0.000000000000000000, -0.000000000000000000, 1.000000000000000000 ) ) ;
#2669 = CARTESIAN_POINT ( 'NONE',  ( 56.65037692655921120, 63.10051614449766078, 2.184720259617097593 ) ) ;
#2670 = FACE_OUTER_BOUND ( 'NONE', #8845, .T. ) ;
#2671 = LINE ( 'NONE', #13374, #13561 ) ;
#2672 = CARTESIAN_POINT ( 'NONE',  ( 54.13287192849676188, 56.29948385550240175, 5.649768623646098220 ) ) ;
#2673 = CARTESIAN_POINT ( 'NONE',  ( 50.02271294988512551, 46.49948385550240459, 7.000000000000000888 ) ) ;
#2674 = CIRCLE ( 'NONE', #6872, 2.055000000000000160 ) ;
#2675 = ADVANCED_FACE ( 'NONE', ( #9369 ), #7371, .F. ) ;
#2676 = CARTESIAN_POINT ( 'NONE',  ( 45.86712807150323812, 51.29948385550240175, -5.649768623646098220 ) ) ;
#2677 = VERTEX_POINT ( 'NONE', #13569 ) ;
#2678 = EDGE_LOOP ( 'NONE', ( #12084, #5636, #1440, #4102 ) ) ;
#2679 = DIRECTION ( 'NONE',  ( -1.000000000000000000, -0.000000000000000000, -0.000000000000000000 ) ) ;
#2680 = ORIENTED_EDGE ( 'NONE', *, *, #4096, .F. ) ;
#2681 = CARTESIAN_POINT ( 'NONE',  ( 6.445379721942640749, -2.463581311471618740, -5.110653333236677476 ) ) ;
#2682 = AXIS2_PLACEMENT_3D ( 'NONE', #10460, #10393, #4172 ) ;
#2683 = VECTOR ( 'NONE', #8505, 1000.000000000000000 ) ;
#2684 = CIRCLE ( 'NONE', #2027, 0.7500000000000000000 ) ;
#2685 = CARTESIAN_POINT ( 'NONE',  ( 6.533910050139696502, -2.950514251728084236, -5.110440592449055686 ) ) ;
#2686 = CARTESIAN_POINT ( 'NONE',  ( 51.97223112728249816, 60.60051614449765367, -5.992620115222793586 ) ) ;
#2687 = CARTESIAN_POINT ( 'NONE',  ( -2.837560373301905643E-16, 0.3423821193871246504, -3.499999999999999556 ) ) ;
#2688 = CARTESIAN_POINT ( 'NONE',  ( 49.97728705011486738, 61.49948385550241170, -8.000000000000001776 ) ) ;
#2689 = CARTESIAN_POINT ( 'NONE',  ( 55.96859303347804371, 60.19948385550240744, 4.306917132069425946 ) ) ;
#2690 = LINE ( 'NONE', #2617, #2475 ) ;
#2691 = CARTESIAN_POINT ( 'NONE',  ( 43.18075615816994173, 63.80051614449766362, 4.924951120819380357 ) ) ;
#2692 = VECTOR ( 'NONE', #2911, 1000.000000000000000 ) ;
#2693 = AXIS2_PLACEMENT_3D ( 'NONE', #13356, #10259, #12398 ) ;
#2694 = ORIENTED_EDGE ( 'NONE', *, *, #2540, .F. ) ;
#2695 = ORIENTED_EDGE ( 'NONE', *, *, #7552, .T. ) ;
#2696 = VERTEX_POINT ( 'NONE', #1890 ) ;
#2697 = ORIENTED_EDGE ( 'NONE', *, *, #8399, .T. ) ;
#2698 = DIRECTION ( 'NONE',  ( -0.000000000000000000, -0.000000000000000000, 1.000000000000000000 ) ) ;
#2699 = FILL_AREA_STYLE ('',( #9275 ) ) ;
#2700 = DIRECTION ( 'NONE',  ( 0.000000000000000000, 0.000000000000000000, 1.000000000000000000 ) ) ;
#2701 = CYLINDRICAL_SURFACE ( 'NONE', #12377, 12.49999999999999645 ) ;
#2702 = DIRECTION ( 'NONE',  ( 0.000000000000000000, 0.000000000000000000, 1.000000000000000000 ) ) ;
#2703 = CARTESIAN_POINT ( 'NONE',  ( 51.92680522751233951, 63.59948385550239891, -6.007379884777223289 ) ) ;
#2704 = CARTESIAN_POINT ( 'NONE',  ( 45.90387839640208512, 52.30051614449766362, -5.676469297603124353 ) ) ;
#2705 = CARTESIAN_POINT ( 'NONE',  ( 58.41169779390614281, 51.00051614449765935, 0.02388180880515032231 ) ) ;
#2706 = VECTOR ( 'NONE', #6733, 1000.000000000000000 ) ;
#2707 = PLANE ( 'NONE',  #681 ) ;
#2708 = CARTESIAN_POINT ( 'NONE',  ( 2.649999999999988365, 15.00000000000001599, 15.00000000000000000 ) ) ;
#2709 = CARTESIAN_POINT ( 'NONE',  ( 43.20883090819742023, 46.20051614449766220, -4.963592699178938972 ) ) ;
#2710 = AXIS2_PLACEMENT_3D ( 'NONE', #13622, #8391, #3128 ) ;
#2712 = ORIENTED_EDGE ( 'NONE', *, *, #9792, .T. ) ;
#2711 = VERTEX_POINT ( 'NONE', #9229 ) ;
#2713 = CARTESIAN_POINT ( 'NONE',  ( 0.000000000000000000, 0.5192545390863916310, -1.000000000000000000 ) ) ;
#2714 = EDGE_CURVE ( 'NONE', #9523, #10506, #3071, .T. ) ;
#2715 = ORIENTED_EDGE ( 'NONE', *, *, #9266, .F. ) ;
#2716 = EDGE_CURVE ( 'NONE', #5028, #3281, #2094, .T. ) ;
#2717 = PLANE ( 'NONE',  #7832 ) ;
#2718 = CARTESIAN_POINT ( 'NONE',  ( -62.49999999999997158, 32.50000000000001421, 15.00000000000000000 ) ) ;
#2719 = EDGE_CURVE ( 'NONE', #11823, #11760, #1819, .T. ) ;
#2720 = EDGE_CURVE ( 'NONE', #4781, #9621, #4114, .T. ) ;
#2721 = DIRECTION ( 'NONE',  ( -9.710251638871368927E-17, -5.969973981896232516E-17, -0.9999999999999997780 ) ) ;
#2722 = CARTESIAN_POINT ( 'NONE',  ( 54.09612160359786515, 55.69948385550240744, -5.676469297603166098 ) ) ;
#2723 = CARTESIAN_POINT ( 'NONE',  ( 52.29715082351547295, 58.39948385550240317, 6.992620115222774047 ) ) ;
#2724 = CARTESIAN_POINT ( 'NONE',  ( 2.649999999999989697, 15.00000000000001599, -9.000000000000001776 ) ) ;
#2725 = FACE_OUTER_BOUND ( 'NONE', #13498, .T. ) ;
#2726 = FACE_OUTER_BOUND ( 'NONE', #7147, .T. ) ;
#2727 = EDGE_CURVE ( 'NONE', #12550, #10183, #4779, .T. ) ;
#2728 = CARTESIAN_POINT ( 'NONE',  ( 44.28664221472221385, 61.90051614449766504, 1.832500667257213722 ) ) ;
#2729 = CARTESIAN_POINT ( 'NONE',  ( 44.28664221472220675, 53.09948385550240602, -1.832500667257165317 ) ) ;
#2730 = CARTESIAN_POINT ( 'NONE',  ( -2.000000000000000000, -6.429618962271402616, -1.000000000000000000 ) ) ;
#2731 = ORIENTED_EDGE ( 'NONE', *, *, #4598, .F. ) ;
#2732 = ORIENTED_EDGE ( 'NONE', *, *, #3011, .T. ) ;
#2733 = ORIENTED_EDGE ( 'NONE', *, *, #9161, .T. ) ;
#2734 = CARTESIAN_POINT ( 'NONE',  ( 5.100000000000002309, 0.000000000000000000, 5.200000000000001066 ) ) ;
#2735 = CARTESIAN_POINT ( 'NONE',  ( 1.925929944387235853E-31, 15.00000000000001599, 15.00000000000000000 ) ) ;
#2736 = ADVANCED_FACE ( 'NONE', ( #3005 ), #11436, .F. ) ;
#2737 = DIRECTION ( 'NONE',  ( 0.000000000000000000, 0.000000000000000000, -1.000000000000000000 ) ) ;
#2738 = EDGE_CURVE ( 'NONE', #2102, #11896, #9569, .T. ) ;
#2739 = CARTESIAN_POINT ( 'NONE',  ( -74.99999999999998579, -2.602085213965210642E-14, 0.000000000000000000 ) ) ;
#2740 = CARTESIAN_POINT ( 'NONE',  ( 4.124214193018075569, -2.028338413290941666, 3.513185186763556622 ) ) ;
#2741 = AXIS2_PLACEMENT_3D ( 'NONE', #7558, #1104, #2087 ) ;
#2742 = CARTESIAN_POINT ( 'NONE',  ( 56.66441430157294690, 60.90051614449766504, -2.141517661632166281 ) ) ;
#2743 = PLANE ( 'NONE',  #3538 ) ;
#2744 = CARTESIAN_POINT ( 'NONE',  ( 53.54508667620424234, 44.70051614449765509, -4.840751629271188961 ) ) ;
#2745 = CARTESIAN_POINT ( 'NONE',  ( -9.999999999999998224, 15.00000000000001776, 15.00000000000000000 ) ) ;
#2746 = AXIS2_PLACEMENT_3D ( 'NONE', #11584, #1115, #13429 ) ;
#2747 = CARTESIAN_POINT ( 'NONE',  ( 52.29715082351547295, 56.39948385550238896, 6.992620115222774047 ) ) ;
#2748 = CARTESIAN_POINT ( 'NONE',  ( 54.09612160359786515, 49.69948385550240744, -5.676469297603166098 ) ) ;
#2749 = AXIS2_PLACEMENT_3D ( 'NONE', #12637, #10221, #13386 ) ;
#2750 = CARTESIAN_POINT ( 'NONE',  ( 52.25172492374522903, 47.59948385550239891, -7.007379884777225953 ) ) ;
#2751 = VECTOR ( 'NONE', #9258, 1000.000000000000000 ) ;
#2752 = ORIENTED_EDGE ( 'NONE', *, *, #8570, .T. ) ;
#2753 = EDGE_LOOP ( 'NONE', ( #2317, #1268, #13413, #2609, #10383 ) ) ;
#2754 = CARTESIAN_POINT ( 'NONE',  ( -2.354826896168714434, -6.962563485461402024, -1.000000000000000000 ) ) ;
#2755 = ORIENTED_EDGE ( 'NONE', *, *, #12525, .T. ) ;
#2756 = DIRECTION ( 'NONE',  ( 1.000000000000000000, 0.000000000000000000, 0.000000000000000000 ) ) ;
#2757 = AXIS2_PLACEMENT_3D ( 'NONE', #12688, #13511, #3023 ) ;
#2758 = EDGE_CURVE ( 'NONE', #2448, #3263, #12059, .T. ) ;
#2759 = CARTESIAN_POINT ( 'NONE',  ( -6.080745460913608902, 0.5192545390863924082, -1.000000000000000000 ) ) ;
#2760 = CARTESIAN_POINT ( 'NONE',  ( 55.71335778527780036, 60.90051614449766504, -1.832500667257213056 ) ) ;
#2761 = CARTESIAN_POINT ( 'NONE',  ( 4.211399257449709665, -2.459727064652517114, -3.751161691472417736 ) ) ;
#2762 = CARTESIAN_POINT ( 'NONE',  ( 54.72065718078924590, 60.29948385550240175, 6.458785618021043895 ) ) ;
#2763 = CARTESIAN_POINT ( 'NONE',  ( 49.97728705011488159, 65.49948385550240459, -7.000000000000000888 ) ) ;
#2764 = DIRECTION ( 'NONE',  ( 0.000000000000000000, 0.000000000000000000, -1.000000000000000000 ) ) ;
#2765 = B_SPLINE_CURVE_WITH_KNOTS ( 'NONE', 3,
 ( #8853, #4492, #13050, #7612, #3595, #465 ),
 .UNSPECIFIED., .F., .F.,
 ( 4, 2, 4 ),
 ( 0.002044882221487524104, 0.003063384235218490244, 0.004081886248949456383 ),
 .UNSPECIFIED. ) ;
#2766 = CARTESIAN_POINT ( 'NONE',  ( 42.39856655714566358, 48.89948385550241028, 2.493737253992119207 ) ) ;
#2767 = ORIENTED_EDGE ( 'NONE', *, *, #8814, .T. ) ;
#2768 = CONTEXT_DEPENDENT_SHAPE_REPRESENTATION ( #2568, #2014 ) ;
#2769 = ORIENTED_EDGE ( 'NONE', *, *, #12174, .F. ) ;
#2770 = ORIENTED_EDGE ( 'NONE', *, *, #12472, .F. ) ;
#2771 = VERTEX_POINT ( 'NONE', #1182 ) ;
#2772 = CARTESIAN_POINT ( 'NONE',  ( 5.991014884144048480, 2.818925648462311528E-15, 4.999999999999999112 ) ) ;
#2773 = CARTESIAN_POINT ( 'NONE',  ( 2.449293598294706513E-15, -20.00000000000000000, 9.000000000000000000 ) ) ;
#2774 =( NAMED_UNIT ( * ) SI_UNIT ( $, .STERADIAN. ) SOLID_ANGLE_UNIT ( ) );
#2775 = FACE_OUTER_BOUND ( 'NONE', #3905, .T. ) ;
#2776 = DIRECTION ( 'NONE',  ( 0.000000000000000000, 0.5000000000000011102, 0.8660254037844379305 ) ) ;
#2777 = FACE_OUTER_BOUND ( 'NONE', #8476, .T. ) ;
#2778 = CARTESIAN_POINT ( 'NONE',  ( 50.02271294988506156, 44.50051614449765935, -6.000000000000000888 ) ) ;
#2779 = CARTESIAN_POINT ( 'NONE',  ( 56.66441430157294690, 50.90051614449766504, -2.141517661632166281 ) ) ;
#2780 = CARTESIAN_POINT ( 'NONE',  ( 56.81924384183006538, 58.80051614449766362, -4.924951120819380357 ) ) ;
#2781 = LINE ( 'NONE', #4792, #6884 ) ;
#2782 = CARTESIAN_POINT ( 'NONE',  ( 2.000000000000000000, 0.000000000000000000, 1.535500000000000087 ) ) ;
#2783 = EDGE_CURVE ( 'NONE', #4363, #9971, #12986, .T. ) ;
#2784 = CARTESIAN_POINT ( 'NONE',  ( 57.60143344285435774, 51.10051614449766078, 2.493737253992045044 ) ) ;
#2786 = ORIENTED_EDGE ( 'NONE', *, *, #13281, .F. ) ;
#2785 = EDGE_LOOP ( 'NONE', ( #2209, #2348, #6141, #5563, #1336, #1370 ) ) ;
#2787 = CARTESIAN_POINT ( 'NONE',  ( 0.3198814748697593746, 4.434118497892183264, -0.3507732604232499107 ) ) ;
#2788 = EDGE_CURVE ( 'NONE', #11948, #6035, #13148, .T. ) ;
#2789 = VERTEX_POINT ( 'NONE', #5559 ) ;
#2790 = CARTESIAN_POINT ( 'NONE',  ( 0.05140428708382594608, 3.841181488860376358, -3.346878500200759277 ) ) ;
#2791 = DIRECTION ( 'NONE',  ( 0.000000000000000000, -0.000000000000000000, 1.000000000000000000 ) ) ;
#2792 = VECTOR ( 'NONE', #6065, 1000.000000000000114 ) ;
#2793 = SHAPE_DEFINITION_REPRESENTATION ( #2547, #180 ) ;
#2794 = CARTESIAN_POINT ( 'NONE',  ( 55.94051828345050836, 63.79948385550240886, -4.345558710429104465 ) ) ;
#2795 = CARTESIAN_POINT ( 'NONE',  ( 49.97728705011488159, 59.49948385550240459, -7.000000000000000888 ) ) ;
#2796 = VECTOR ( 'NONE', #10173, 1000.000000000000000 ) ;
#2797 = CARTESIAN_POINT ( 'NONE',  ( 0.000000000000000000, -3.031088913245531202, 1.750000000000006439 ) ) ;
#2798 = DIRECTION ( 'NONE',  ( -0.000000000000000000, 1.000000000000000000, -0.000000000000000000 ) ) ;
#2799 = CARTESIAN_POINT ( 'NONE',  ( 6.371919382990604674, 1.972754410575522588, 5.108792907957607099 ) ) ;
#2800 = CARTESIAN_POINT ( 'NONE',  ( 46.45491332379576477, 63.70051614449766930, 4.840751629271188961 ) ) ;
#2801 = CARTESIAN_POINT ( 'NONE',  ( 44.30067958973596376, 52.89948385550241028, 1.875703265242204099 ) ) ;
#2802 = DIRECTION ( 'NONE',  ( 0.000000000000000000, -0.000000000000000000, 1.000000000000000000 ) ) ;
#2803 = ADVANCED_FACE ( 'NONE', ( #8672 ), #10867, .T. ) ;
#2804 = ORIENTED_EDGE ( 'NONE', *, *, #417, .F. ) ;
#2805 = ADVANCED_FACE ( 'NONE', ( #12934 ), #12867, .T. ) ;
#2806 = EDGE_LOOP ( 'NONE', ( #2145, #12723 ) ) ;
#2807 = VERTEX_POINT ( 'NONE', #7498 ) ;
#2808 = CARTESIAN_POINT ( 'NONE',  ( 4.132952817037859106, -2.031684012687264396, -3.518979934899745032 ) ) ;
#2809 = CARTESIAN_POINT ( 'NONE',  ( 6.092449800118089343, 3.827241605637482724, -3.371023086194387286 ) ) ;
#2810 = CARTESIAN_POINT ( 'NONE',  ( 6.390820841722131718, -2.823237767533154141, -5.110008744785255352 ) ) ;
#2811 = PRESENTATION_STYLE_ASSIGNMENT (( #7928 ) ) ;
#2812 = CARTESIAN_POINT ( 'NONE',  ( 55.94051828345050836, 45.79948385550240886, -4.345558710429104465 ) ) ;
#2813 = CARTESIAN_POINT ( 'NONE',  ( 2.449293598294706513E-15, -20.00000000000000000, -23.00000000000000000 ) ) ;
#2814 = CARTESIAN_POINT ( 'NONE',  ( 51.97223112728249816, 44.60051614449766078, -5.992620115222793586 ) ) ;
#2815 = CYLINDRICAL_SURFACE ( 'NONE', #4981, 2.649999999999988365 ) ;
#2816 = CARTESIAN_POINT ( 'NONE',  ( 45.86712807150323812, 57.29948385550240175, -5.649768623646098220 ) ) ;
#2817 = CARTESIAN_POINT ( 'NONE',  ( 45.86712807150323812, 53.29948385550240886, -5.649768623646098220 ) ) ;
#2818 = EDGE_LOOP ( 'NONE', ( #8993, #7956, #9062, #9327 ) ) ;
#2819 = CARTESIAN_POINT ( 'NONE',  ( 54.13287192849676188, 48.29948385550240175, 5.649768623646098220 ) ) ;
#2820 = EDGE_CURVE ( 'NONE', #12042, #3434, #10604, .T. ) ;
#2821 = VERTEX_POINT ( 'NONE', #9702 ) ;
#2822 = ORIENTED_EDGE ( 'NONE', *, *, #2051, .F. ) ;
#2823 = PLANE ( 'NONE',  #1491 ) ;
#2824 = ORIENTED_EDGE ( 'NONE', *, *, #6056, .F. ) ;
#2825 = CARTESIAN_POINT ( 'NONE',  ( 0.2174200650117528444, 2.185595227304856891, -3.214438021527932676 ) ) ;
#2826 = CARTESIAN_POINT ( 'NONE',  ( 5.686050877451574337, -5.768780236673276995, -1.000000000000000000 ) ) ;
#2827 = CARTESIAN_POINT ( 'NONE',  ( 48.02776887271750184, 59.60051614449765367, 5.992620115222795363 ) ) ;
#2828=STYLED_ITEM('',(#13698),#10251);
#2829 = CARTESIAN_POINT ( 'NONE',  ( 4.000000000000000000, -1.700175430507292473, -3.320327275037661785 ) ) ;
#2830 = CARTESIAN_POINT ( 'NONE',  ( 57.60143344285433642, 57.89948385550241028, -2.493737253992118319 ) ) ;
#2831 = DIRECTION ( 'NONE',  ( 0.000000000000000000, 0.000000000000000000, 1.000000000000000000 ) ) ;
#2832 = DIRECTION ( 'NONE',  ( 1.000000000000000000, 0.000000000000000000, 0.000000000000000000 ) ) ;
#2833 = CARTESIAN_POINT ( 'NONE',  ( 42.38452918213188525, 47.09948385550240602, -2.450534656007040013 ) ) ;
#2834 = EDGE_LOOP ( 'NONE', ( #10782, #13044, #1897, #7724 ) ) ;
#2835 = ORIENTED_EDGE ( 'NONE', *, *, #9989, .T. ) ;
#2836 = APPLICATION_CONTEXT ( 'automotive_design' ) ;
#2837 = ORIENTED_EDGE ( 'NONE', *, *, #7332, .T. ) ;
#2838 = AXIS2_PLACEMENT_3D ( 'NONE', #3097, #3859, #8084 ) ;
#2839 = CARTESIAN_POINT ( 'NONE',  ( 45.60000000000000142, 0.000000000000000000, 0.000000000000000000 ) ) ;
#2840 = FACE_OUTER_BOUND ( 'NONE', #9132, .T. ) ;
#2841 =( NAMED_UNIT ( * ) PLANE_ANGLE_UNIT ( ) SI_UNIT ( $, .RADIAN. ) );
#2842 = CARTESIAN_POINT ( 'NONE',  ( 3.972066048304756514, 2.740530939476224059, -2.384802634787894338 ) ) ;
#2843 = CARTESIAN_POINT ( 'NONE',  ( 4.071447262713890680, -4.041451884327386779, 0.000000000000000000 ) ) ;
#2844 = CARTESIAN_POINT ( 'NONE',  ( 55.71335778527780036, 44.90051614449765793, -1.832500667257213056 ) ) ;
#2845 = CARTESIAN_POINT ( 'NONE',  ( 44.05948171654945611, 54.20051614449765509, -4.345558710429044069 ) ) ;
#2846 = CARTESIAN_POINT ( 'NONE',  ( 47.42335538002180328, 60.40051614449765793, -8.007379884777206414 ) ) ;
#2847 = CIRCLE ( 'NONE', #10121, 1.500000000000001554 ) ;
#2848 = DIRECTION ( 'NONE',  ( -1.000000000000000000, 0.000000000000000000, 0.000000000000000000 ) ) ;
#2849 = CARTESIAN_POINT ( 'NONE',  ( 57.60143344285435774, 53.10051614449767499, 2.493737253992045044 ) ) ;
#2850 = AXIS2_PLACEMENT_3D ( 'NONE', #8753, #11789, #9651 ) ;
#2852 = ORIENTED_EDGE ( 'NONE', *, *, #10894, .T. ) ;
#2851 = ORIENTED_EDGE ( 'NONE', *, *, #267, .F. ) ;
#2853 = DIRECTION ( 'NONE',  ( 0.000000000000000000, 0.000000000000000000, -1.000000000000000000 ) ) ;
#2854 = VERTEX_POINT ( 'NONE', #160 ) ;
#2855 =( GEOMETRIC_REPRESENTATION_CONTEXT ( 3 ) GLOBAL_UNCERTAINTY_ASSIGNED_CONTEXT ( ( #11500 ) ) GLOBAL_UNIT_ASSIGNED_CONTEXT ( ( #13300, #7865, #6964 ) ) REPRESENTATION_CONTEXT ( 'NONE', 'WORKASPACE' ) );
#2856 = ORIENTED_EDGE ( 'NONE', *, *, #8833, .T. ) ;
#2857 = CARTESIAN_POINT ( 'NONE',  ( -4.999999999999998224, -20.00000000000000000, -8.999999999999998224 ) ) ;
#2858 = CARTESIAN_POINT ( 'NONE',  ( -2.354826896168714434, -6.962563485461402024, 0.000000000000000000 ) ) ;
#2859 = PRODUCT_CONTEXT ( 'NONE', #11835, 'mechanical' ) ;
#2860 = CARTESIAN_POINT ( 'NONE',  ( 44.03140696652192787, 63.19948385550240744, -4.306917132069425058 ) ) ;
#2861 = EDGE_CURVE ( 'NONE', #12021, #6051, #7411, .T. ) ;
#2862 = CARTESIAN_POINT ( 'NONE',  ( 44.05948171654949874, 58.79948385550240175, 4.345558710429104465 ) ) ;
#2863 = LINE ( 'NONE', #9298, #13057 ) ;
#2864 = DIRECTION ( 'NONE',  ( 1.000000000000000000, 0.000000000000000000, 0.000000000000000000 ) ) ;
#2865 = ORIENTED_EDGE ( 'NONE', *, *, #2122, .F. ) ;
#2866 = LINE ( 'NONE', #10263, #12636 ) ;
#2867 = CARTESIAN_POINT ( 'NONE',  ( 52.29715082351538769, 48.60051614449766788, -6.992620115222796251 ) ) ;
#2868 = CARTESIAN_POINT ( 'NONE',  ( 55.71335778527780747, 52.09948385550241312, 1.832500667257165983 ) ) ;
#2869 = AXIS2_PLACEMENT_3D ( 'NONE', #5399, #1995, #12704 ) ;
#2870 = DIRECTION ( 'NONE',  ( -0.000000000000000000, -0.000000000000000000, 1.000000000000000000 ) ) ;
#2871 = ORIENTED_EDGE ( 'NONE', *, *, #6489, .F. ) ;
#2872 = ORIENTED_EDGE ( 'NONE', *, *, #2369, .F. ) ;
#2873 = ORIENTED_EDGE ( 'NONE', *, *, #4058, .F. ) ;
#2874 = CARTESIAN_POINT ( 'NONE',  ( 4.158413352280807551, -2.044871626972826650, -3.541821552872960410 ) ) ;
#2875 = CARTESIAN_POINT ( 'NONE',  ( 2.449293598294706513E-15, -20.00000000000000000, -8.999999999999998224 ) ) ;
#2876 = CARTESIAN_POINT ( 'NONE',  ( 6.212068001623061164, -3.310128279683368202, -4.266689640017852447 ) ) ;
#2877 = AXIS2_PLACEMENT_3D ( 'NONE', #996, #6356, #5107 ) ;
#2878 = SURFACE_SIDE_STYLE ('',( #9244 ) ) ;
#2879 = CARTESIAN_POINT ( 'NONE',  ( 43.33558569842703179, 47.09948385550240602, -2.141517661632099223 ) ) ;
#2880 = FILL_AREA_STYLE ('',( #7101 ) ) ;
#2881 = CARTESIAN_POINT ( 'NONE',  ( 6.506892073925696351, 2.992473431090949543, -5.000000000000000000 ) ) ;
#2882 = CARTESIAN_POINT ( 'NONE',  ( 55.69932041026405045, 45.10051614449766788, 1.875703265242156359 ) ) ;
#2883 = DIRECTION ( 'NONE',  ( -1.000000000000000000, 0.000000000000000000, 1.224646799147353207E-16 ) ) ;
#2884 = CARTESIAN_POINT ( 'NONE',  ( 50.02271294988512551, 58.49948385550241170, 7.000000000000000888 ) ) ;
#2885 = CARTESIAN_POINT ( 'NONE',  ( 47.70284917648453415, 51.39948385550238896, -6.992620115222774047 ) ) ;
#2886 = ADVANCED_FACE ( 'NONE', ( #11703 ), #12669, .T. ) ;
#2887 = ORIENTED_EDGE ( 'NONE', *, *, #1196, .T. ) ;
#2888 = CARTESIAN_POINT ( 'NONE',  ( 54.13287192849676188, 50.29948385550240175, 5.649768623646098220 ) ) ;
#2889 = TOROIDAL_SURFACE ( 'NONE', #11502, 7.900000000000002132, 0.5999999999999979794 ) ;
#2890 = ORIENTED_EDGE ( 'NONE', *, *, #10531, .T. ) ;
#2891 = CARTESIAN_POINT ( 'NONE',  ( 20.00000000000000000, -14.99999999999999289, -23.00000000000000000 ) ) ;
#2892 = ORIENTED_EDGE ( 'NONE', *, *, #8641, .F. ) ;
#2893 = CARTESIAN_POINT ( 'NONE',  ( 4.158413352280808439, 2.044871626972822209, 3.541821552872961298 ) ) ;
#2894 = LINE ( 'NONE', #4072, #6089 ) ;
#2895 = DIRECTION ( 'NONE',  ( 1.000000000000000000, 0.000000000000000000, -0.000000000000000000 ) ) ;
#2896 = EDGE_CURVE ( 'NONE', #3939, #9950, #5494, .T. ) ;
#2897 = AXIS2_PLACEMENT_3D ( 'NONE', #1214, #10631, #6366 ) ;
#2898 = CARTESIAN_POINT ( 'NONE',  ( 44.28664221472221385, 61.90051614449766504, 1.832500667257213722 ) ) ;
#2899 = EDGE_CURVE ( 'NONE', #3196, #5220, #6596, .T. ) ;
#2900 = DIRECTION ( 'NONE',  ( -0.000000000000000000, -0.000000000000000000, 1.000000000000000000 ) ) ;
#2901 = CARTESIAN_POINT ( 'NONE',  ( 52.57664461997811856, 61.59948385550240602, -8.007379884777229506 ) ) ;
#2902 = CARTESIAN_POINT ( 'NONE',  ( 44.05948171654949874, 64.79948385550240175, 4.345558710429105354 ) ) ;
#2903 = DIRECTION ( 'NONE',  ( -0.9989677110047504582, -0.04542589977017007230, 1.386346192018204258E-14 ) ) ;
#2904 = CARTESIAN_POINT ( 'NONE',  ( 45.31609314410967926, 52.69948385550240744, 6.485486291978119766 ) ) ;
#2905 = EDGE_LOOP ( 'NONE', ( #5183, #1140, #4287, #10711, #12022, #9220, #8658, #6657, #6582 ) ) ;
#2906 = VECTOR ( 'NONE', #9763, 1000.000000000000000 ) ;
#2907 = VERTEX_POINT ( 'NONE', #11906 ) ;
#2908 = ORIENTED_EDGE ( 'NONE', *, *, #3602, .T. ) ;
#2909 = FACE_BOUND ( 'NONE', #6769, .T. ) ;
#2910 =( NAMED_UNIT ( * ) PLANE_ANGLE_UNIT ( ) SI_UNIT ( $, .RADIAN. ) );
#2911 = DIRECTION ( 'NONE',  ( -1.000000000000000000, -0.000000000000000000, -0.000000000000000000 ) ) ;
#2912 = FACE_BOUND ( 'NONE', #1738, .T. ) ;
#2913 = EDGE_CURVE ( 'NONE', #7674, #940, #1149, .T. ) ;
#2914 = FACE_OUTER_BOUND ( 'NONE', #899, .T. ) ;
#2915 = CARTESIAN_POINT ( 'NONE',  ( 49.97728705011488870, 63.49948385550241170, -6.000000000000000888 ) ) ;
#2916 = CARTESIAN_POINT ( 'NONE',  ( 47.74827507625470702, 50.40051614449765793, -7.007379884777204637 ) ) ;
#2917 = CARTESIAN_POINT ( 'NONE',  ( 41.58830220609386430, 58.00051614449765935, -0.02388180880514929535 ) ) ;
#2918 = VECTOR ( 'NONE', #6042, 1000.000000000000000 ) ;
#2919 = AXIS2_PLACEMENT_3D ( 'NONE', #771, #5022, #9228 ) ;
#2920 = CARTESIAN_POINT ( 'NONE',  ( 3.951447005078448260, 1.347150628109122339, -3.499999999999999112 ) ) ;
#2921 = CARTESIAN_POINT ( 'NONE',  ( 45.27934281921082516, 51.70051614449765509, 6.458785618021089192 ) ) ;
#2923 = EDGE_LOOP ( 'NONE', ( #166, #1303, #5281, #9689 ) ) ;
#2922 = ORIENTED_EDGE ( 'NONE', *, *, #11155, .F. ) ;
#2924 = ADVANCED_FACE ( 'NONE', ( #2159 ), #2932, .T. ) ;
#2925 = ORIENTED_EDGE ( 'NONE', *, *, #10083, .F. ) ;
#2926 = PRODUCT_DEFINITION_CONTEXT ( 'detailed design', #1403, 'design' ) ;
#2927 = ORIENTED_EDGE ( 'NONE', *, *, #5526, .F. ) ;
#2928 = CARTESIAN_POINT ( 'NONE',  ( 0.000000000000000000, -3.031088913245531202, 1.750000000000006439 ) ) ;
#2929 = CIRCLE ( 'NONE', #3589, 4.999999999999999112 ) ;
#2930 = CARTESIAN_POINT ( 'NONE',  ( -4.799999999999999822, 5.878304635907294211E-16, 0.000000000000000000 ) ) ;
#2931 = DIRECTION ( 'NONE',  ( 1.000000000000000000, 0.000000000000000000, 0.000000000000000000 ) ) ;
#2932 = CONICAL_SURFACE ( 'NONE', #1368, 5.371010071662833063, 1.221730476396037490 ) ;
#2933 = PRODUCT_CONTEXT ( 'NONE', #2836, 'mechanical' ) ;
#2934 = CARTESIAN_POINT ( 'NONE',  ( 56.30877334542961421, 45.99948385550240459, -0.02388180880520959434 ) ) ;
#2935 = CARTESIAN_POINT ( 'NONE',  ( 44.05948171654949874, 60.79948385550240886, 4.345558710429104465 ) ) ;
#2936 = CARTESIAN_POINT ( 'NONE',  ( -22.14999999999999858, -19.99999999999999289, -23.00000000000000000 ) ) ;
#2937 = CARTESIAN_POINT ( 'NONE',  ( 0.000000000000000000, -0.8865213383406694847, 1.535500000000001419 ) ) ;
#2938 = CARTESIAN_POINT ( 'NONE',  ( -6.000000000000013323, -7.009618943233427935, -9.000000000000000000 ) ) ;
#2939 = CARTESIAN_POINT ( 'NONE',  ( 57.36023556966787851, 53.00051614449765225, 0.02388180880515038476 ) ) ;
#2940 = CARTESIAN_POINT ( 'NONE',  ( 44.91013252490152752, 54.79948385550240175, 3.727524721679198461 ) ) ;
#2941 = CARTESIAN_POINT ( 'NONE',  ( 54.89903213687075834, 44.74560054925188268, -5.000000000000007105 ) ) ;
#2942 = EDGE_LOOP ( 'NONE', ( #5221, #6786, #12087, #4366 ) ) ;
#2943 = CIRCLE ( 'NONE', #1825, 5.000000000000000888 ) ;
#2944 = LINE ( 'NONE', #7168, #4339 ) ;
#2945 = ORIENTED_EDGE ( 'NONE', *, *, #754, .T. ) ;
#2946 = ORIENTED_EDGE ( 'NONE', *, *, #12963, .T. ) ;
#2947 = CARTESIAN_POINT ( 'NONE',  ( 4.142654963991852846, -2.035398498734352746, -3.525413613457307971 ) ) ;
#2948 = FACE_OUTER_BOUND ( 'NONE', #13091, .T. ) ;
#2949 = DIRECTION ( 'NONE',  ( -1.000000000000000000, -4.082155997157843695E-16, 0.000000000000000000 ) ) ;
#2950 = CLOSED_SHELL ( 'NONE', ( #6174, #8344, #9664, #6098, #2981, #7491, #8600, #10497, #7205, #10910, #2300, #9930, #10273, #9322, #11759, #1937, #1728, #8370, #10770, #3896, #7071, #10494, #5349, #10066, #7769, #664, #7458, #4338, #6200, #6808, #7135, #9712, #2282, #990, #13011, #6166, #10063, #4236, #5363, #5115 ) ) ;
#2951 = SHAPE_REPRESENTATION_RELATIONSHIP ( 'NONE' , 'NONE' ,  #9196, #870 ) ;
#2952 = CARTESIAN_POINT ( 'NONE',  ( 0.000000000000000000, -1.773042676681341856, 2.276824562219559311E-15 ) ) ;
#2953 = DIRECTION ( 'NONE',  ( -1.000000000000000000, -0.000000000000000000, -0.000000000000000000 ) ) ;
#2954 = DIRECTION ( 'NONE',  ( -9.858538378746663627E-23, 5.031452844637890958E-23, -1.000000000000000000 ) ) ;
#2955 = CARTESIAN_POINT ( 'NONE',  ( 53.54508667620428497, 64.29948385550240175, 4.840751629271157874 ) ) ;
#2956 = CARTESIAN_POINT ( 'NONE',  ( 2.449293598294706513E-15, -20.00000000000000000, -9.000000000000000000 ) ) ;
#2957 = CARTESIAN_POINT ( 'NONE',  ( 49.97728705011488159, 59.49948385550240459, -7.000000000000000888 ) ) ;
#2958 = CARTESIAN_POINT ( 'NONE',  ( 54.13287192849676188, 52.29948385550240886, 5.649768623646098220 ) ) ;
#2959 = ORIENTED_EDGE ( 'NONE', *, *, #12763, .T. ) ;
#2960 = CARTESIAN_POINT ( 'NONE',  ( 57.36023556966787851, 47.99948385550239038, -0.02388180880522424582 ) ) ;
#2961 = ORIENTED_EDGE ( 'NONE', *, *, #585, .F. ) ;
#2962 = DIRECTION ( 'NONE',  ( 0.000000000000000000, 0.000000000000000000, -1.000000000000000000 ) ) ;
#2963 = ORIENTED_EDGE ( 'NONE', *, *, #2212, .F. ) ;
#2964 = ADVANCED_FACE ( 'NONE', ( #10795 ), #1313, .F. ) ;
#2965 = CIRCLE ( 'NONE', #12043, 5.000000000000000888 ) ;
#2966 = CARTESIAN_POINT ( 'NONE',  ( 4.175572532730931208, 2.061029303918050726, 3.569807470274392713 ) ) ;
#2967 = DIRECTION ( 'NONE',  ( -1.224646799147353207E-16, 0.000000000000000000, -1.000000000000000000 ) ) ;
#2968 = CARTESIAN_POINT ( 'NONE',  ( 54.09612160359786515, 45.69948385550240744, -5.676469297603166098 ) ) ;
#2969 = CARTESIAN_POINT ( 'NONE',  ( 50.02271294988506156, 60.50051614449766646, -6.000000000000000888 ) ) ;
#2970 = CARTESIAN_POINT ( 'NONE',  ( -4.000000000000000000, 0.000000000000000000, 0.000000000000000000 ) ) ;
#2971 = CARTESIAN_POINT ( 'NONE',  ( 57.61547081786812896, 58.09948385550241312, 2.450534656007040901 ) ) ;
#2972 = CARTESIAN_POINT ( 'NONE',  ( 0.000000000000000000, 0.000000000000000000, -0.2800830152838844622 ) ) ;
#2973 = EDGE_CURVE ( 'NONE', #12054, #614, #3164, .T. ) ;
#2974 = VECTOR ( 'NONE', #8259, 1000.000000000000000 ) ;
#2975 = EDGE_CURVE ( 'NONE', #7759, #10697, #5977, .T. ) ;
#2976 = CARTESIAN_POINT ( 'NONE',  ( 41.58830220609386430, 46.99948385550239749, 0.02388180880523263147 ) ) ;
#2977 = EDGE_CURVE ( 'NONE', #7203, #11927, #7905, .T. ) ;
#2978 = ORIENTED_EDGE ( 'NONE', *, *, #7070, .T. ) ;
#2979 = AXIS2_PLACEMENT_3D ( 'NONE', #4884, #11020, #1751 ) ;
#2980 = ORIENTED_EDGE ( 'NONE', *, *, #6378, .T. ) ;
#2981 = ADVANCED_FACE ( 'NONE', ( #4725 ), #5835, .T. ) ;
#2982 = ORIENTED_EDGE ( 'NONE', *, *, #2544, .T. ) ;
#2983 = DIRECTION ( 'NONE',  ( 0.000000000000000000, 0.000000000000000000, 1.000000000000000000 ) ) ;
#2984 = VECTOR ( 'NONE', #5047, 1000.000000000000000 ) ;
#2985 = CARTESIAN_POINT ( 'NONE',  ( 2.649999999999988365, 15.00000000000001599, 15.00000000000000000 ) ) ;
#2986 = DIRECTION ( 'NONE',  ( -0.000000000000000000, 0.000000000000000000, -1.000000000000000000 ) ) ;
#2987 = CARTESIAN_POINT ( 'NONE',  ( -20.00000000000000000, -25.00000000000000000, -20.00000000000000000 ) ) ;
#2988 = CARTESIAN_POINT ( 'NONE',  ( 44.28664221472220675, 61.09948385550241312, -1.832500667257165317 ) ) ;
#2989 = CARTESIAN_POINT ( 'NONE',  ( 47.70284917648459810, 51.60051614449765367, 6.992620115222797139 ) ) ;
#2990 = CARTESIAN_POINT ( 'NONE',  ( 57.60143344285435774, 59.10051614449766078, 2.493737253992045044 ) ) ;
#2991 = CARTESIAN_POINT ( 'NONE',  ( -4.000000000000000000, -1.680117682357936904, -3.316611593218794951 ) ) ;
#2992 = CARTESIAN_POINT ( 'NONE',  ( 47.42335538002180328, 48.40051614449766504, -8.007379884777206414 ) ) ;
#2994 = ORIENTED_EDGE ( 'NONE', *, *, #8052, .T. ) ;
#2993 = EDGE_LOOP ( 'NONE', ( #11127, #3922, #8118, #2980 ) ) ;
#2995 = ORIENTED_EDGE ( 'NONE', *, *, #2540, .T. ) ;
#2996 = VERTEX_POINT ( 'NONE', #416 ) ;
#2997 = CARTESIAN_POINT ( 'NONE',  ( -1.438549683741723797E-15, -3.375361811986503202, 1.153701847711634532 ) ) ;
#2998 = DIRECTION ( 'NONE',  ( 1.040834085586083310E-14, -1.000000000000000000, 0.000000000000000000 ) ) ;
#2999 = DIRECTION ( 'NONE',  ( -0.000000000000000000, -0.000000000000000000, 1.000000000000000000 ) ) ;
#3000 = SHAPE_DEFINITION_REPRESENTATION ( #1459, #10521 ) ;
#3001 = CARTESIAN_POINT ( 'NONE',  ( 43.34962307344081012, 62.89948385550241028, 2.184720259617164650 ) ) ;
#3002 = CARTESIAN_POINT ( 'NONE',  ( 44.03140696652193498, 57.19948385550239323, -4.306917132069424170 ) ) ;
#3003 = CARTESIAN_POINT ( 'NONE',  ( 52.29715082351538769, 60.60051614449764656, -6.992620115222796251 ) ) ;
#3004 = CARTESIAN_POINT ( 'NONE',  ( -1.000000000000000000, -14.00000000000000000, 8.999999999999998224 ) ) ;
#3005 = FACE_OUTER_BOUND ( 'NONE', #762, .T. ) ;
#3006 = CARTESIAN_POINT ( 'NONE',  ( 54.76112626223286384, 45.00000000000007816, -5.734953493745535091 ) ) ;
#3007 = CARTESIAN_POINT ( 'NONE',  ( 44.03140696652198471, 51.80051614449766362, 4.306917132069485454 ) ) ;
#3008 = CARTESIAN_POINT ( 'NONE',  ( 50.02271294988511841, 52.49948385550241170, 6.000000000000000888 ) ) ;
#3009 = CARTESIAN_POINT ( 'NONE',  ( 0.000000000000000000, 0.000000000000000000, 0.000000000000000000 ) ) ;
#3010 = ORIENTED_EDGE ( 'NONE', *, *, #1689, .T. ) ;
#3011 = EDGE_CURVE ( 'NONE', #4812, #8256, #8875, .T. ) ;
#3012 = LINE ( 'NONE', #5564, #7937 ) ;
#3013 = ORIENTED_EDGE ( 'NONE', *, *, #8473, .F. ) ;
#3014 = ORIENTED_EDGE ( 'NONE', *, *, #7162, .F. ) ;
#3015 = DIRECTION ( 'NONE',  ( -1.000000000000000000, -0.000000000000000000, -0.000000000000000000 ) ) ;
#3016 = VECTOR ( 'NONE', #835, 1000.000000000000114 ) ;
#3017 = CARTESIAN_POINT ( 'NONE',  ( 6.204460410672268722, 3.831267809383005041, -3.364049496745006529 ) ) ;
#3018 = PLANE ( 'NONE',  #6000 ) ;
#3019 =( NAMED_UNIT ( * ) SI_UNIT ( $, .STERADIAN. ) SOLID_ANGLE_UNIT ( ) );
#3020 = CARTESIAN_POINT ( 'NONE',  ( 49.97728705011488159, 45.49948385550240459, -7.000000000000000888 ) ) ;
#3021 = CARTESIAN_POINT ( 'NONE',  ( -4.141042297810615835, 2.227970268150415656, -3.687027686973619822 ) ) ;
#3022 = CARTESIAN_POINT ( 'NONE',  ( 44.28664221472220675, 65.09948385550239891, -1.832500667257165317 ) ) ;
#3023 = DIRECTION ( 'NONE',  ( -1.000000000000000000, 0.000000000000000000, 0.000000000000000000 ) ) ;
#3024 = CARTESIAN_POINT ( 'NONE',  ( 45.86712807150323812, 65.29948385550241596, -5.649768623646098220 ) ) ;
#3025 = CARTESIAN_POINT ( 'NONE',  ( 47.74827507625478518, 54.59948385550239180, 7.007379884777227730 ) ) ;
#3026 = ORIENTED_EDGE ( 'NONE', *, *, #9719, .T. ) ;
#3027 = CARTESIAN_POINT ( 'NONE',  ( 47.74827507625478518, 52.59948385550239180, 7.007379884777227730 ) ) ;
#3028 = ORIENTED_EDGE ( 'NONE', *, *, #4761, .F. ) ;
#3029 = DIRECTION ( 'NONE',  ( 0.000000000000000000, 0.000000000000000000, 1.000000000000000000 ) ) ;
#3030 = ORIENTED_EDGE ( 'NONE', *, *, #6297, .F. ) ;
#3031 = CARTESIAN_POINT ( 'NONE',  ( 2.449293598294706513E-15, -20.00000000000000000, -20.00000000000000000 ) ) ;
#3032 = CARTESIAN_POINT ( 'NONE',  ( 1.925929944387235853E-31, 15.00000000000001599, 9.000000000000000000 ) ) ;
#3033 = CARTESIAN_POINT ( 'NONE',  ( 52.29715082351547295, 46.39948385550240317, 6.992620115222774047 ) ) ;
#3034 = CARTESIAN_POINT ( 'NONE',  ( 47.74827507625469281, 46.40051614449764372, -7.007379884777203749 ) ) ;
#3035 = DIRECTION ( 'NONE',  ( 1.000000000000000000, 0.000000000000000000, 0.000000000000000000 ) ) ;
#3036 = CARTESIAN_POINT ( 'NONE',  ( 57.61547081786812896, 64.09948385550239891, 2.450534656007040901 ) ) ;
#3037 = CARTESIAN_POINT ( 'NONE',  ( 13.99999999999999822, 0.000000000000000000, 0.000000000000000000 ) ) ;
#3038 = DIRECTION ( 'NONE',  ( -0.000000000000000000, 0.000000000000000000, 1.000000000000000000 ) ) ;
#3039 = EDGE_CURVE ( 'NONE', #10021, #3041, #6864, .T. ) ;
#3040 = CARTESIAN_POINT ( 'NONE',  ( 52.57664461997811856, 47.59948385550239891, -8.007379884777229506 ) ) ;
#3041 = VERTEX_POINT ( 'NONE', #8943 ) ;
#3042 = ORIENTED_EDGE ( 'NONE', *, *, #3183, .F. ) ;
#3043 = ORIENTED_EDGE ( 'NONE', *, *, #2433, .F. ) ;
#3044 = CARTESIAN_POINT ( 'NONE',  ( 54.31203442848995877, 44.90264883920728778, -4.999999999999999112 ) ) ;
#3045 = PRESENTATION_LAYER_ASSIGNMENT (  '', '', ( #9005 ) ) ;
#3046 = DIRECTION ( 'NONE',  ( 1.000000000000000000, 0.000000000000000000, 0.000000000000000000 ) ) ;
#3047 = CARTESIAN_POINT ( 'NONE',  ( -62.49999999999997158, 32.50000000000001421, -15.00000000000000000 ) ) ;
#3048 = CARTESIAN_POINT ( 'NONE',  ( 0.000000000000000000, 0.000000000000000000, 0.000000000000000000 ) ) ;
#3049 = CARTESIAN_POINT ( 'NONE',  ( 55.11794222512599362, 48.80051614449767072, -3.688883143319583446 ) ) ;
#3050 = CARTESIAN_POINT ( 'NONE',  ( 54.09612160359792199, 59.30051614449766362, 5.676469297603124353 ) ) ;
#3051 = CARTESIAN_POINT ( 'NONE',  ( 58.41169779390614281, 57.00051614449766646, 0.02388180880515032231 ) ) ;
#3052 = CARTESIAN_POINT ( 'NONE',  ( -62.49999999999997158, 32.50000000000001421, 15.00000000000000178 ) ) ;
#3053 = CARTESIAN_POINT ( 'NONE',  ( 50.02271294988505446, 50.50051614449765935, -8.000000000000001776 ) ) ;
#3054 = VECTOR ( 'NONE', #7812, 1000.000000000000000 ) ;
#3056 = ORIENTED_EDGE ( 'NONE', *, *, #9519, .F. ) ;
#3055 = ORIENTED_EDGE ( 'NONE', *, *, #3685, .T. ) ;
#3057 = ORIENTED_EDGE ( 'NONE', *, *, #7332, .F. ) ;
#3058 = UNCERTAINTY_MEASURE_WITH_UNIT (LENGTH_MEASURE( 1.000000000000000082E-05 ), #12513, 'distance_accuracy_value', 'NONE');
#3059 = ORIENTED_EDGE ( 'NONE', *, *, #5886, .T. ) ;
#3060 = ORIENTED_EDGE ( 'NONE', *, *, #11753, .T. ) ;
#3061 = FILL_AREA_STYLE_COLOUR ( '', #7687 ) ;
#3062 = CARTESIAN_POINT ( 'NONE',  ( -4.999999999999998224, -20.00000000000000000, 15.00000000000000355 ) ) ;
#3063 = CARTESIAN_POINT ( 'NONE',  ( -4.000000000000000000, -2.309401076758512694, -3.433295621305382461 ) ) ;
#3064 = CARTESIAN_POINT ( 'NONE',  ( 54.09612160359786515, 61.69948385550240744, -5.676469297603166098 ) ) ;
#3065 = AXIS2_PLACEMENT_3D ( 'NONE', #12740, #3282, #6479 ) ;
#3066 = CARTESIAN_POINT ( 'NONE',  ( 54.13287192849676188, 64.29948385550241596, 5.649768623646098220 ) ) ;
#3067 = EDGE_CURVE ( 'NONE', #690, #1489, #13074, .T. ) ;
#3068 = CARTESIAN_POINT ( 'NONE',  ( 43.34962307344078880, 58.10051614449766078, -2.184720259617096705 ) ) ;
#3069 = ADVANCED_FACE ( 'NONE', ( #3750 ), #11067, .F. ) ;
#3070 = DIRECTION ( 'NONE',  ( -1.000000000000000000, -0.000000000000000000, -0.000000000000000000 ) ) ;
#3071 = LINE ( 'NONE', #6277, #12931 ) ;
#3072 = CARTESIAN_POINT ( 'NONE',  ( 53.94396537754659704, 44.99999999999997158, -6.362703256440709332 ) ) ;
#3073 = CARTESIAN_POINT ( 'NONE',  ( 44.05948171654945611, 52.20051614449764799, -4.345558710429044069 ) ) ;
#3074 = CARTESIAN_POINT ( 'NONE',  ( 50.02271294988511841, 60.49948385550240459, 6.000000000000000888 ) ) ;
#3075 = CARTESIAN_POINT ( 'NONE',  ( -4.000000000000000000, 2.309401076758498483, -3.433295621305379353 ) ) ;
#3076 = ADVANCED_FACE ( 'NONE', ( #1523 ), #9900, .T. ) ;
#3077 = ORIENTED_EDGE ( 'NONE', *, *, #13406, .T. ) ;
#3078 =( GEOMETRIC_REPRESENTATION_CONTEXT ( 3 ) GLOBAL_UNCERTAINTY_ASSIGNED_CONTEXT ( ( #3700 ) ) GLOBAL_UNIT_ASSIGNED_CONTEXT ( ( #6003, #10342, #9445 ) ) REPRESENTATION_CONTEXT ( 'NONE', 'WORKASPACE' ) );
#3079 = CARTESIAN_POINT ( 'NONE',  ( 2.449293598294706513E-15, -20.00000000000000000, 9.000000000000000000 ) ) ;
#3080 = CIRCLE ( 'NONE', #10790, 12.49999999999999645 ) ;
#3081 = ORIENTED_EDGE ( 'NONE', *, *, #272, .T. ) ;
#3082 = ORIENTED_EDGE ( 'NONE', *, *, #5188, .F. ) ;
#3083 = CARTESIAN_POINT ( 'NONE',  ( 2.449293598294706513E-15, -20.00000000000000000, -23.00000000000000000 ) ) ;
#3084 = VECTOR ( 'NONE', #98, 1000.000000000000000 ) ;
#3085 = DIRECTION ( 'NONE',  ( -9.858538378746663627E-23, 5.031452844637890958E-23, -1.000000000000000000 ) ) ;
#3086 = CARTESIAN_POINT ( 'NONE',  ( 6.506891485183659896, -2.992470280394939675, 5.000000000000000000 ) ) ;
#3087 =( NAMED_UNIT ( * ) PLANE_ANGLE_UNIT ( ) SI_UNIT ( $, .RADIAN. ) );
#3088 = LINE ( 'NONE', #2952, #7700 ) ;
#3089 = CARTESIAN_POINT ( 'NONE',  ( -74.99999999999997158, 32.50000000000001421, 9.999999999999998224 ) ) ;
#3090 = CARTESIAN_POINT ( 'NONE',  ( 51.92680522751238925, 49.40051614449766504, 6.007379884777208190 ) ) ;
#3091 = DIRECTION ( 'NONE',  ( -9.710251638871371392E-17, -5.969973981896233748E-17, -1.000000000000000000 ) ) ;
#3092 = CARTESIAN_POINT ( 'NONE',  ( 56.65037692655918988, 63.89948385550239607, -2.184720259617163762 ) ) ;
#3093 = CARTESIAN_POINT ( 'NONE',  ( 42.63976443033212860, 54.99948385550241170, 0.02388180880522514787 ) ) ;
#3094 = CIRCLE ( 'NONE', #12580, 4.000000000000000000 ) ;
#3095 = ORIENTED_EDGE ( 'NONE', *, *, #503, .F. ) ;
#3096 = ORIENTED_EDGE ( 'NONE', *, *, #4024, .T. ) ;
#3097 = CARTESIAN_POINT ( 'NONE',  ( -1.250000000000000000, -6.429618962271402616, 0.000000000000000000 ) ) ;
#3098 = VECTOR ( 'NONE', #4821, 1000.000000000000000 ) ;
#3099 = LINE ( 'NONE', #2057, #2751 ) ;
#3100 = DIRECTION ( 'NONE',  ( -0.000000000000000000, 0.000000000000000000, 1.000000000000000000 ) ) ;
#3101 = DIRECTION ( 'NONE',  ( 0.000000000000000000, 1.776356839400250267E-15, 1.000000000000000000 ) ) ;
#3102 = CARTESIAN_POINT ( 'NONE',  ( 56.65037692655918988, 45.89948385550240317, -2.184720259617163762 ) ) ;
#3103 = APPLICATION_CONTEXT ( 'automotive_design' ) ;
#3104 = CARTESIAN_POINT ( 'NONE',  ( 43.33558569842706021, 49.90051614449766504, 2.141517661632167169 ) ) ;
#3105 = FACE_BOUND ( 'NONE', #1609, .T. ) ;
#3106 = EDGE_CURVE ( 'NONE', #9468, #9956, #144, .T. ) ;
#3107 = CARTESIAN_POINT ( 'NONE',  ( 54.13287192849676188, 46.29948385550240886, 5.649768623646098220 ) ) ;
#3108 = COLOUR_RGB ( '',0.8941176470588234615, 0.8941176470588234615, 0.8941176470588234615 ) ;
#3109 = CARTESIAN_POINT ( 'NONE',  ( 32.49999999999998579, 5.000000000000018652, 5.000000000000003553 ) ) ;
#3110 = VECTOR ( 'NONE', #6711, 1000.000000000000000 ) ;
#3111 = CARTESIAN_POINT ( 'NONE',  ( 54.72065718078924590, 58.29948385550240886, 6.458785618021043895 ) ) ;
#3112 = ORIENTED_EDGE ( 'NONE', *, *, #2465, .F. ) ;
#3113 = EDGE_LOOP ( 'NONE', ( #7723, #4903, #5534, #149, #4501 ) ) ;
#3114 = DIRECTION ( 'NONE',  ( -1.000000000000000000, 0.000000000000000000, 0.000000000000000000 ) ) ;
#3115 = CARTESIAN_POINT ( 'NONE',  ( 4.211140560182196957, -2.431303136016555122, -3.745885042887436622 ) ) ;
#3116 = CARTESIAN_POINT ( 'NONE',  ( 6.355827204229362870, -3.436818823786764288, -4.264647808192651546 ) ) ;
#3117 = CARTESIAN_POINT ( 'NONE',  ( 2.742827927723449299, 3.035229711104609596, -3.433252694550591233 ) ) ;
#3118 = CARTESIAN_POINT ( 'NONE',  ( 55.69932041026405045, 47.10051614449766078, 1.875703265242156359 ) ) ;
#3119 = CARTESIAN_POINT ( 'NONE',  ( 56.66441430157294690, 56.90051614449766504, -2.141517661632166281 ) ) ;
#3120 = CARTESIAN_POINT ( 'NONE',  ( 52.62207051974829852, 62.60051614449765367, -7.992620115222797139 ) ) ;
#3121 = DIRECTION ( 'NONE',  ( 0.000000000000000000, 0.000000000000000000, 1.000000000000000000 ) ) ;
#3122 = CARTESIAN_POINT ( 'NONE',  ( 50.02271294988505446, 56.50051614449767357, -8.000000000000001776 ) ) ;
#3123 = CIRCLE ( 'NONE', #5124, 0.2000000000000000944 ) ;
#3124 = PRODUCT_DEFINITION_SHAPE ( 'NONE', 'NONE',  #10642 ) ;
#3125 = EDGE_LOOP ( 'NONE', ( #7895, #2865, #12528, #567 ) ) ;
#3126 = ORIENTED_EDGE ( 'NONE', *, *, #3820, .T. ) ;
#3127 = ORIENTED_EDGE ( 'NONE', *, *, #5203, .F. ) ;
#3128 = DIRECTION ( 'NONE',  ( 0.000000000000000000, 0.000000000000000000, 1.000000000000000000 ) ) ;
#3129 = CARTESIAN_POINT ( 'NONE',  ( 5.560781378645575757, 0.000000000000000000, -4.000000000000000000 ) ) ;
#3130 = EDGE_CURVE ( 'NONE', #7203, #11305, #10998, .T. ) ;
#3131 = CARTESIAN_POINT ( 'NONE',  ( 4.071447262713887127, 2.020725942163686284, -3.499999999999999556 ) ) ;
#3132 = CARTESIAN_POINT ( 'NONE',  ( 0.000000000000000000, 0.000000000000000000, 0.000000000000000000 ) ) ;
#3133 = AXIS2_PLACEMENT_3D ( 'NONE', #7644, #299, #4526 ) ;
#3134 = CARTESIAN_POINT ( 'NONE',  ( 48.02776887271745210, 47.39948385550241028, -5.992620115222778487 ) ) ;
#3135 = CIRCLE ( 'NONE', #7992, 1.610000000000000098 ) ;
#3136 = DIRECTION ( 'NONE',  ( 0.000000000000000000, 0.000000000000000000, 1.000000000000000000 ) ) ;
#3137 = AXIS2_PLACEMENT_3D ( 'NONE', #6761, #573, #9994 ) ;
#3138 = B_SPLINE_CURVE_WITH_KNOTS ( 'NONE', 3,
 ( #3305, #3439, #5395, #6561 ),
 .UNSPECIFIED., .F., .F.,
 ( 4, 4 ),
 ( 0.000000000000000000, 0.002080789711329296236 ),
 .UNSPECIFIED. ) ;
#3139 = CARTESIAN_POINT ( 'NONE',  ( 57.61547081786810764, 44.90051614449765793, -2.450534656007114176 ) ) ;
#3140 = CARTESIAN_POINT ( 'NONE',  ( 4.000000000000000000, -1.084202172485504434E-14, -3.142992957459231906 ) ) ;
#3141 = CARTESIAN_POINT ( 'NONE',  ( -0.1481481481481481122, -4.797713218419819903, 0.000000000000000000 ) ) ;
#3142 = CARTESIAN_POINT ( 'NONE',  ( 3.950241966887845457, 3.393956070637746514, -1.121495646998088569 ) ) ;
#3143 = CARTESIAN_POINT ( 'NONE',  ( 43.34962307344078880, 50.10051614449766078, -2.184720259617096705 ) ) ;
#3144 = CARTESIAN_POINT ( 'NONE',  ( 55.08986747509847248, 59.79948385550240175, -3.727524721679197572 ) ) ;
#3145 = DIRECTION ( 'NONE',  ( 0.000000000000000000, 0.000000000000000000, 1.000000000000000000 ) ) ;
#3146 = ADVANCED_FACE ( 'NONE', ( #5767 ), #9967, .T. ) ;
#3147 = VERTEX_POINT ( 'NONE', #10178 ) ;
#3148 = AXIS2_PLACEMENT_3D ( 'NONE', #5589, #10445, #3185 ) ;
#3149 = DIRECTION ( 'NONE',  ( 0.000000000000000000, 0.000000000000000000, 1.000000000000000000 ) ) ;
#3150 = ADVANCED_FACE ( 'NONE', ( #682 ), #8240, .T. ) ;
#3151 = ORIENTED_EDGE ( 'NONE', *, *, #5779, .T. ) ;
#3152 = CARTESIAN_POINT ( 'NONE',  ( 20.00000000000000000, -20.00000000000000000, -12.00000000000000000 ) ) ;
#3153 = EDGE_CURVE ( 'NONE', #919, #10854, #8801, .T. ) ;
#3154 = LINE ( 'NONE', #5445, #6745 ) ;
#3155 = CARTESIAN_POINT ( 'NONE',  ( 4.175326769692854434, 2.060699556488891027, -3.569236330973487803 ) ) ;
#3156 = PRESENTATION_STYLE_ASSIGNMENT (( #993 ) ) ;
#3157 = CARTESIAN_POINT ( 'NONE',  ( 54.09612160359786515, 53.69948385550240744, -5.676469297603166098 ) ) ;
#3158 = CARTESIAN_POINT ( 'NONE',  ( 49.99999999999997158, 45.00000000000001421, -6.500000000000004441 ) ) ;
#3159 = CARTESIAN_POINT ( 'NONE',  ( 44.91013252490150620, 52.20051614449766220, -3.727524721679154940 ) ) ;
#3160 = CARTESIAN_POINT ( 'NONE',  ( 0.02944718078674397194, -0.6813962075909725247, -3.500000000000000000 ) ) ;
#3161 = DIRECTION ( 'NONE',  ( 0.000000000000000000, 1.000000000000000000, 0.000000000000000000 ) ) ;
#3162 = CARTESIAN_POINT ( 'NONE',  ( 56.66441430157296821, 62.09948385550239891, 2.141517661632100111 ) ) ;
#3163 = CARTESIAN_POINT ( 'NONE',  ( 54.09612160359786515, 57.69948385550240744, -5.676469297603166098 ) ) ;
#3164 = CIRCLE ( 'NONE', #10873, 12.49999999999999645 ) ;
#3165 = VERTEX_POINT ( 'NONE', #9420 ) ;
#3166 = VERTEX_POINT ( 'NONE', #6186 ) ;
#3167 = ADVANCED_FACE ( 'NONE', ( #10381 ), #6891, .F. ) ;
#3168 = CLOSED_SHELL ( 'NONE', ( #5681, #5378, #3734, #5913, #6032, #13101 ) ) ;
#3169 = CARTESIAN_POINT ( 'NONE',  ( 0.000000000000000000, 0.000000000000000000, -20.00000000000000000 ) ) ;
#3170 = EDGE_CURVE ( 'NONE', #10837, #331, #11981, .T. ) ;
#3171 = CARTESIAN_POINT ( 'NONE',  ( 6.165086708099646984, -33.67449106481162602, 9.000000000000000000 ) ) ;
#3172 = DIRECTION ( 'NONE',  ( 0.000000000000000000, -1.000000000000000000, 0.000000000000000000 ) ) ;
#3173 = DIRECTION ( 'NONE',  ( 0.000000000000000000, 0.000000000000000000, 1.000000000000000000 ) ) ;
#3174 = CARTESIAN_POINT ( 'NONE',  ( 42.63976443033212860, 46.00051614449766646, -0.02388180880514948964 ) ) ;
#3175 = DIRECTION ( 'NONE',  ( 0.000000000000000000, 1.000000000000000000, -9.783878858594328898E-16 ) ) ;
#3176 = CARTESIAN_POINT ( 'NONE',  ( 42.38452918213188525, 63.09948385550240602, -2.450534656007040013 ) ) ;
#3177 = CARTESIAN_POINT ( 'NONE',  ( 0.000000000000000000, 0.000000000000000000, 0.000000000000000000 ) ) ;
#3178 = CARTESIAN_POINT ( 'NONE',  ( 47.42335538002188144, 56.59948385550239891, 8.007379884777233059 ) ) ;
#3179 = AXIS2_PLACEMENT_3D ( 'NONE', #11237, #4962, #711 ) ;
#3180 = ORIENTED_EDGE ( 'NONE', *, *, #11088, .T. ) ;
#3181 = ADVANCED_FACE ( 'NONE', ( #9284 ), #13339, .F. ) ;
#3182 = ORIENTED_EDGE ( 'NONE', *, *, #10900, .F. ) ;
#3183 = EDGE_CURVE ( 'NONE', #10299, #9221, #11093, .T. ) ;
#3184 = DIRECTION ( 'NONE',  ( 1.000000000000000000, 0.000000000000000000, 0.000000000000000000 ) ) ;
#3185 = DIRECTION ( 'NONE',  ( 1.000000000000000000, 0.000000000000000000, 0.000000000000000000 ) ) ;
#3186 = CARTESIAN_POINT ( 'NONE',  ( 75.00000000000001421, -39.99999999999998579, -20.00000000000000000 ) ) ;
#3187 = LINE ( 'NONE', #6383, #1672 ) ;
#3188 = CARTESIAN_POINT ( 'NONE',  ( 55.08986747509849380, 49.20051614449766220, 3.727524721679155384 ) ) ;
#3189 = CARTESIAN_POINT ( 'NONE',  ( 54.13287192849671214, 56.70051614449766220, -5.649768623646139964 ) ) ;
#3190 = AXIS2_PLACEMENT_3D ( 'NONE', #11990, #10040, #12057 ) ;
#3191 = CARTESIAN_POINT ( 'NONE',  ( 52.62207051974839089, 48.39948385550240317, 7.992620115222770494 ) ) ;
#3192 = CARTESIAN_POINT ( 'NONE',  ( 4.175813232069150338, -4.122719923832746325, 2.362127131240695889E-16 ) ) ;
#3193 = AXIS2_PLACEMENT_3D ( 'NONE', #6554, #10755, #5454 ) ;
#3194 = CARTESIAN_POINT ( 'NONE',  ( 42.39856655714564226, 58.10051614449765367, -2.493737253992044156 ) ) ;
#3195 = AXIS2_PLACEMENT_3D ( 'NONE', #12897, #9801, #1071 ) ;
#3196 = VERTEX_POINT ( 'NONE', #5003 ) ;
#3197 = EDGE_LOOP ( 'NONE', ( #5861, #685, #4051, #1018 ) ) ;
#3198 = ORIENTED_EDGE ( 'NONE', *, *, #7704, .T. ) ;
#3199 = AXIS2_PLACEMENT_3D ( 'NONE', #11749, #7538, #10647 ) ;
#3200 = CARTESIAN_POINT ( 'NONE',  ( -1.240299975428134203E-15, -4.736529461165891242, -3.681130640444276292 ) ) ;
#3201 = LINE ( 'NONE', #8456, #10986 ) ;
#3202 = CARTESIAN_POINT ( 'NONE',  ( 32.49999999999998579, 45.00000000000001421, 5.000000000000003553 ) ) ;
#3203 = CIRCLE ( 'NONE', #4085, 6.080745460913608902 ) ;
#3204 = LINE ( 'NONE', #4370, #8653 ) ;
#3205 = FACE_OUTER_BOUND ( 'NONE', #10609, .T. ) ;
#3206 = CARTESIAN_POINT ( 'NONE',  ( 51.92680522751233951, 51.59948385550240602, -6.007379884777223289 ) ) ;
#3207 = DIRECTION ( 'NONE',  ( 0.000000000000000000, 0.000000000000000000, 1.000000000000000000 ) ) ;
#3208 = EDGE_CURVE ( 'NONE', #2278, #4659, #3592, .T. ) ;
#3209 = CARTESIAN_POINT ( 'NONE',  ( 43.33558569842706021, 63.90051614449765793, 2.141517661632167169 ) ) ;
#3210 = FACE_OUTER_BOUND ( 'NONE', #7045, .T. ) ;
#3211 = DIRECTION ( 'NONE',  ( 1.000000000000000000, 0.000000000000000000, 0.000000000000000000 ) ) ;
#3212 = VECTOR ( 'NONE', #10478, 1000.000000000000000 ) ;
#3213 = DIRECTION ( 'NONE',  ( 0.000000000000000000, 0.000000000000000000, 1.000000000000000000 ) ) ;
#3214 = CARTESIAN_POINT ( 'NONE',  ( 55.96859303347802239, 54.80051614449764230, -4.306917132069484566 ) ) ;
#3215 = CARTESIAN_POINT ( 'NONE',  ( 51.97223112728254790, 60.39948385550241028, 5.992620115222778487 ) ) ;
#3216 = CARTESIAN_POINT ( 'NONE',  ( -4.799999999999999822, 5.878304635907294211E-16, -1.000000000000000000 ) ) ;
#3217 = EDGE_CURVE ( 'NONE', #9824, #11777, #11758, .T. ) ;
#3218 = ORIENTED_EDGE ( 'NONE', *, *, #13008, .F. ) ;
#3219 = FACE_OUTER_BOUND ( 'NONE', #7190, .T. ) ;
#3220 = ORIENTED_EDGE ( 'NONE', *, *, #587, .F. ) ;
#3221 = LINE ( 'NONE', #989, #5070 ) ;
#3222 = DIRECTION ( 'NONE',  ( 0.000000000000000000, 0.000000000000000000, 1.000000000000000000 ) ) ;
#3223 = CARTESIAN_POINT ( 'NONE',  ( 4.104070371397485317, 2.023683613428364225, -3.505122836902508698 ) ) ;
#3224 = CARTESIAN_POINT ( 'NONE',  ( 0.000000000000000000, 0.000000000000000000, 0.000000000000000000 ) ) ;
#3225 = CARTESIAN_POINT ( 'NONE',  ( 45.86712807150323812, 49.29948385550240175, -5.649768623646098220 ) ) ;
#3226 = CARTESIAN_POINT ( 'NONE',  ( 2.449293598294706513E-15, -20.00000000000000000, 9.000000000000000000 ) ) ;
#3227 = CARTESIAN_POINT ( 'NONE',  ( 43.69122665457040000, 54.00051614449765935, -0.02388180880515696977 ) ) ;
#3228 = EDGE_CURVE ( 'NONE', #10246, #5348, #11338, .T. ) ;
#3229 = CARTESIAN_POINT ( 'NONE',  ( 6.367873360227559232, -5.773502691896263528, 0.000000000000000000 ) ) ;
#3230 = CARTESIAN_POINT ( 'NONE',  ( 57.36023556966787851, 63.99948385550241881, -0.02388180880522424582 ) ) ;
#3231 = SURFACE_STYLE_FILL_AREA ( #12817 ) ;
#3232 = CARTESIAN_POINT ( 'NONE',  ( 42.63976443033212860, 62.99948385550241170, 0.02388180880522514787 ) ) ;
#3233 = EDGE_CURVE ( 'NONE', #7327, #9150, #8320, .T. ) ;
#3234 = ORIENTED_EDGE ( 'NONE', *, *, #623, .F. ) ;
#3235 = CIRCLE ( 'NONE', #3672, 2.649999999999985700 ) ;
#3236 = AXIS2_PLACEMENT_3D ( 'NONE', #6346, #1967, #2036 ) ;
#3237 = EDGE_LOOP ( 'NONE', ( #3059, #7039, #9360, #8788 ) ) ;
#3238 = LINE ( 'NONE', #11864, #7262 ) ;
#3239 = CARTESIAN_POINT ( 'NONE',  ( 1.171083334267915221, -24.65495046420793201, 9.000000000000000000 ) ) ;
#3240 = FACE_OUTER_BOUND ( 'NONE', #5268, .T. ) ;
#3241 = LINE ( 'NONE', #12762, #9605 ) ;
#3242 = CARTESIAN_POINT ( 'NONE',  ( 44.03140696652193498, 49.19948385550240744, -4.306917132069424170 ) ) ;
#3243 = CARTESIAN_POINT ( 'NONE',  ( 45.86712807150329496, 45.70051614449766220, 5.649768623646139964 ) ) ;
#3244 = CARTESIAN_POINT ( 'NONE',  ( 75.00000000000000000, 40.00000000000000000, 10.00000000000000000 ) ) ;
#3245 = CARTESIAN_POINT ( 'NONE',  ( 44.05948171654949874, 46.79948385550238754, 4.345558710429105354 ) ) ;
#3246 = EDGE_CURVE ( 'NONE', #331, #10837, #4038, .T. ) ;
#3247 = AXIS2_PLACEMENT_3D ( 'NONE', #4020, #7350, #8515 ) ;
#3248 = DIRECTION ( 'NONE',  ( -0.000000000000000000, -1.000000000000000000, -0.000000000000000000 ) ) ;
#3249 = ADVANCED_FACE ( 'NONE', ( #9147 ), #12203, .T. ) ;
#3250 = CARTESIAN_POINT ( 'NONE',  ( 54.72065718078924590, 56.29948385550240886, 6.458785618021043895 ) ) ;
#3251 = EDGE_CURVE ( 'NONE', #13462, #12709, #10005, .T. ) ;
#3252 = ORIENTED_EDGE ( 'NONE', *, *, #12347, .T. ) ;
#3253 = ORIENTED_EDGE ( 'NONE', *, *, #3692, .T. ) ;
#3254 = CARTESIAN_POINT ( 'NONE',  ( 6.367873360227558344, 5.773502691896261751, 0.000000000000000000 ) ) ;
#3255 = DIRECTION ( 'NONE',  ( -1.000000000000000000, 0.000000000000000000, 0.000000000000000000 ) ) ;
#3256 = DIRECTION ( 'NONE',  ( -0.000000000000000000, -0.000000000000000000, 1.000000000000000000 ) ) ;
#3257 = CARTESIAN_POINT ( 'NONE',  ( 44.30067958973594955, 48.10051614449766078, -1.875703265242155693 ) ) ;
#3258 = CARTESIAN_POINT ( 'NONE',  ( 52.25172492374528588, 61.40051614449765793, 7.007379884777204637 ) ) ;
#3259 = CARTESIAN_POINT ( 'NONE',  ( 42.38452918213188525, 47.09948385550240602, -2.450534656007040013 ) ) ;
#3260 = CARTESIAN_POINT ( 'NONE',  ( 3.961551342853837809, 2.319461885623310682, 2.982574167880912341 ) ) ;
#3261 = B_SPLINE_CURVE_WITH_KNOTS ( 'NONE', 3,
 ( #4796, #8116, #9082, #3826, #11072, #4868, #1527, #12256 ),
 .UNSPECIFIED., .F., .F.,
 ( 4, 2, 2, 4 ),
 ( 2.465131517390770070E-07, 0.001183067374689869946, 0.001774477805458935659, 0.002365888236228001588 ),
 .UNSPECIFIED. ) ;
#3262 = CARTESIAN_POINT ( 'NONE',  ( 47.42335538002180328, 54.40051614449765793, -8.007379884777206414 ) ) ;
#3263 = VERTEX_POINT ( 'NONE', #5071 ) ;
#3264 = ORIENTED_EDGE ( 'NONE', *, *, #1348, .T. ) ;
#3265 = EDGE_LOOP ( 'NONE', ( #8290, #11231, #5908, #5824 ) ) ;
#3266 = FACE_OUTER_BOUND ( 'NONE', #4135, .T. ) ;
#3267 =( LENGTH_UNIT ( ) NAMED_UNIT ( * ) SI_UNIT ( .MILLI., .METRE. ) );
#3268 = LINE ( 'NONE', #5426, #3537 ) ;
#3269 = DIRECTION ( 'NONE',  ( -0.9989677110047502362, -0.04542589977017699732, 6.931730960091013400E-15 ) ) ;
#3270 =( NAMED_UNIT ( * ) PLANE_ANGLE_UNIT ( ) SI_UNIT ( $, .RADIAN. ) );
#3271 = CARTESIAN_POINT ( 'NONE',  ( 44.30067958973596376, 50.89948385550240317, 1.875703265242204099 ) ) ;
#3272 = DIRECTION ( 'NONE',  ( 1.000000000000000000, 0.000000000000000000, 0.000000000000000000 ) ) ;
#3273 = CARTESIAN_POINT ( 'NONE',  ( 57.60143344285435774, 45.10051614449766788, 2.493737253992045044 ) ) ;
#3274 = CARTESIAN_POINT ( 'NONE',  ( 6.355324643801635531, -1.972141403783270075, 5.108685331087992942 ) ) ;
#3275 = CARTESIAN_POINT ( 'NONE',  ( -18.00000000000000355, -19.99999999999999289, -20.00000000000000000 ) ) ;
#3276 = CARTESIAN_POINT ( 'NONE',  ( 42.63976443033212860, 56.00051614449765935, -0.02388180880514948964 ) ) ;
#3277 = CARTESIAN_POINT ( 'NONE',  ( 46.45491332379572924, 59.29948385550240886, -4.840751629271157874 ) ) ;
#3278 = LINE ( 'NONE', #11244, #1189 ) ;
#3279 = ORIENTED_EDGE ( 'NONE', *, *, #11433, .F. ) ;
#3280 = CARTESIAN_POINT ( 'NONE',  ( 1.000000000000002442, -20.00000000000000000, 8.999999999999998224 ) ) ;
#3281 = VERTEX_POINT ( 'NONE', #8580 ) ;
#3282 = DIRECTION ( 'NONE',  ( -0.000000000000000000, -0.000000000000000000, -1.000000000000000000 ) ) ;
#3283 = VECTOR ( 'NONE', #11253, 1000.000000000000000 ) ;
#3284 = EDGE_CURVE ( 'NONE', #11391, #6039, #12639, .T. ) ;
#3285 = CARTESIAN_POINT ( 'NONE',  ( -62.49999999999997158, 32.50000000000001421, -10.00000000000000178 ) ) ;
#3286 = DIRECTION ( 'NONE',  ( 1.000000000000000000, 0.000000000000000000, 0.000000000000000000 ) ) ;
#3287 = CIRCLE ( 'NONE', #11893, 15.00000000000000000 ) ;
#3288 = CARTESIAN_POINT ( 'NONE',  ( 43.33558569842703179, 51.09948385550240602, -2.141517661632099223 ) ) ;
#3289 = CARTESIAN_POINT ( 'NONE',  ( 0.6937372685066666156, -4.453844082567737672, -3.610536846335894445 ) ) ;
#3290 = CARTESIAN_POINT ( 'NONE',  ( 51.92680522751238925, 53.40051614449765793, 6.007379884777208190 ) ) ;
#3291 = DIRECTION ( 'NONE',  ( -9.710251638871371392E-17, -5.969973981896234981E-17, -1.000000000000000000 ) ) ;
#3292 = DIRECTION ( 'NONE',  ( 0.000000000000000000, 0.000000000000000000, 1.000000000000000000 ) ) ;
#3293 = CARTESIAN_POINT ( 'NONE',  ( 6.436591462021358012, -5.789018756751932671, 5.527293451046372024E-16 ) ) ;
#3294 = CARTESIAN_POINT ( 'NONE',  ( 47.74827507625478518, 62.59948385550240602, 7.007379884777227730 ) ) ;
#3295 = DIRECTION ( 'NONE',  ( 0.000000000000000000, -1.073081856240829552E-16, -1.000000000000000000 ) ) ;
#3296 = VERTEX_POINT ( 'NONE', #8519 ) ;
#3297 = AXIS2_PLACEMENT_3D ( 'NONE', #4668, #9721, #2444 ) ;
#3298 = CIRCLE ( 'NONE', #12126, 5.000000000000007994 ) ;
#3299 = UNCERTAINTY_MEASURE_WITH_UNIT (LENGTH_MEASURE( 1.000000000000000082E-05 ), #3506, 'distance_accuracy_value', 'NONE');
#3300 = VERTEX_POINT ( 'NONE', #7481 ) ;
#3301 = VERTEX_POINT ( 'NONE', #8449 ) ;
#3302 = FACE_OUTER_BOUND ( 'NONE', #12491, .T. ) ;
#3303 = DIRECTION ( 'NONE',  ( 0.000000000000000000, 0.000000000000000000, 1.000000000000000000 ) ) ;
#3304 =( GEOMETRIC_REPRESENTATION_CONTEXT ( 3 ) GLOBAL_UNCERTAINTY_ASSIGNED_CONTEXT ( ( #3058 ) ) GLOBAL_UNIT_ASSIGNED_CONTEXT ( ( #12513, #12583, #185 ) ) REPRESENTATION_CONTEXT ( 'NONE', 'WORKASPACE' ) );
#3305 = CARTESIAN_POINT ( 'NONE',  ( 4.175813232069148562, -2.061359961916374051, -3.570380186727397653 ) ) ;
#3306 = DIRECTION ( 'NONE',  ( 1.000000000000000000, 0.000000000000000000, -0.000000000000000000 ) ) ;
#3307 = CARTESIAN_POINT ( 'NONE',  ( 49.97728705011488159, 51.49948385550240459, -7.000000000000000888 ) ) ;
#3308 = CARTESIAN_POINT ( 'NONE',  ( 45.90387839640208512, 46.30051614449766362, -5.676469297603124353 ) ) ;
#3309 = DIRECTION ( 'NONE',  ( -1.000000000000000000, 0.000000000000000000, 0.000000000000000000 ) ) ;
#3310 = EDGE_CURVE ( 'NONE', #757, #1421, #12783, .T. ) ;
#3311 = CARTESIAN_POINT ( 'NONE',  ( 49.97728705011486738, 63.49948385550241170, -8.000000000000001776 ) ) ;
#3312 = PLANE ( 'NONE',  #7041 ) ;
#3313 = PRODUCT_DEFINITION_FORMATION_WITH_SPECIFIED_SOURCE ( 'ANY', '', #12721, .NOT_KNOWN. ) ;
#3314 = CARTESIAN_POINT ( 'NONE',  ( 42.38452918213188525, 55.09948385550241312, -2.450534656007040013 ) ) ;
#3315 = AXIS2_PLACEMENT_3D ( 'NONE', #3226, #5037, #2107 ) ;
#3316 = ADVANCED_FACE ( 'NONE', ( #3326 ), #8315, .F. ) ;
#3317 = ORIENTED_EDGE ( 'NONE', *, *, #11597, .F. ) ;
#3318 = VERTEX_POINT ( 'NONE', #11889 ) ;
#3319 = CARTESIAN_POINT ( 'NONE',  ( 8.759913291900572219, -32.17636723815373756, -9.000000000000000000 ) ) ;
#3320 = EDGE_CURVE ( 'NONE', #4810, #3920, #695, .T. ) ;
#3321 = EDGE_CURVE ( 'NONE', #3999, #3926, #9342, .T. ) ;
#3322 = CARTESIAN_POINT ( 'NONE',  ( 45.60000000000000142, 0.000000000000000000, 0.000000000000000000 ) ) ;
#3323 = CARTESIAN_POINT ( 'NONE',  ( 44.88205777487401349, 47.80051614449764941, 3.688883143319584779 ) ) ;
#3324 = CARTESIAN_POINT ( 'NONE',  ( 55.94051828345054389, 59.20051614449765509, 4.345558710429044957 ) ) ;
#3325 = CARTESIAN_POINT ( 'NONE',  ( 49.97728705011495265, 63.50051614449765935, 8.000000000000001776 ) ) ;
#3326 = FACE_OUTER_BOUND ( 'NONE', #6919, .T. ) ;
#3327 = CARTESIAN_POINT ( 'NONE',  ( 45.31609314410960820, 54.30051614449765651, -6.485486291978072693 ) ) ;
#3328 = EDGE_LOOP ( 'NONE', ( #6851, #7021, #2945, #2887 ) ) ;
#3329 = VERTEX_POINT ( 'NONE', #6452 ) ;
#3330 = ORIENTED_EDGE ( 'NONE', *, *, #10658, .F. ) ;
#3331 = EDGE_LOOP ( 'NONE', ( #9117, #10285, #6836, #2680, #3234, #8758, #8426, #4013, #8427 ) ) ;
#3332 = VECTOR ( 'NONE', #10774, 1000.000000000000000 ) ;
#3333 = CARTESIAN_POINT ( 'NONE',  ( -2.682243648011671588, -3.070208061305317759, -0.04852650426602272971 ) ) ;
#3334 = SURFACE_SIDE_STYLE ('',( #10927 ) ) ;
#3335 = CARTESIAN_POINT ( 'NONE',  ( 4.050480423730737911, -1.376911654797406070, 3.567926555162024282 ) ) ;
#3336 = CARTESIAN_POINT ( 'NONE',  ( 62.49999999999998579, 20.00000000000001421, -15.00000000000000000 ) ) ;
#3337 = DIRECTION ( 'NONE',  ( -1.000000000000000000, 0.000000000000000000, -0.000000000000000000 ) ) ;
#3338 = CARTESIAN_POINT ( 'NONE',  ( 55.69932041026404335, 51.89948385550241028, -1.875703265242203432 ) ) ;
#3339 = CARTESIAN_POINT ( 'NONE',  ( 45.90387839640214196, 62.69948385550240744, 5.676469297603166098 ) ) ;
#3340 = CARTESIAN_POINT ( 'NONE',  ( 49.97728705011495265, 47.50051614449765935, 8.000000000000001776 ) ) ;
#3341 = VECTOR ( 'NONE', #10824, 1000.000000000000000 ) ;
#3342 = CARTESIAN_POINT ( 'NONE',  ( 3.734041964264196878, -16.98388816369253362, -8.999999999999996447 ) ) ;
#3343 = DIRECTION ( 'NONE',  ( 0.000000000000000000, 0.000000000000000000, 1.000000000000000000 ) ) ;
#3344 = EDGE_CURVE ( 'NONE', #11691, #12157, #10654, .T. ) ;
#3345 = CARTESIAN_POINT ( 'NONE',  ( 54.13287192849671214, 56.70051614449766220, -5.649768623646139964 ) ) ;
#3346 = CARTESIAN_POINT ( 'NONE',  ( 44.91013252490152752, 56.79948385550240175, 3.727524721679198461 ) ) ;
#3347 = ORIENTED_EDGE ( 'NONE', *, *, #11556, .T. ) ;
#3348 = FACE_OUTER_BOUND ( 'NONE', #8041, .T. ) ;
#3349 = ORIENTED_EDGE ( 'NONE', *, *, #6379, .T. ) ;
#3350 = CARTESIAN_POINT ( 'NONE',  ( 6.506987859255518813, 2.925375531177291766, 5.066899051217865768 ) ) ;
#3351 = AXIS2_PLACEMENT_3D ( 'NONE', #7533, #10568, #4283 ) ;
#3352 = CARTESIAN_POINT ( 'NONE',  ( 1.171083334267915221, -24.65495046420793201, 9.999999999999998224 ) ) ;
#3353 = AXIS2_PLACEMENT_3D ( 'NONE', #10621, #6487, #3428 ) ;
#3354 = CARTESIAN_POINT ( 'NONE',  ( -4.000000000000000000, -2.309401076758515803, -0.4999999999999995559 ) ) ;
#3355 = CARTESIAN_POINT ( 'NONE',  ( 55.94051828345050836, 53.79948385550238754, -4.345558710429104465 ) ) ;
#3356 = CARTESIAN_POINT ( 'NONE',  ( 0.000000000000000000, 0.000000000000000000, 0.000000000000000000 ) ) ;
#3357 = CARTESIAN_POINT ( 'NONE',  ( 53.54508667620424234, 52.70051614449766220, -4.840751629271188961 ) ) ;
#3358 = FACE_OUTER_BOUND ( 'NONE', #7641, .T. ) ;
#3359 = PLANE ( 'NONE',  #1505 ) ;
#3360 = CARTESIAN_POINT ( 'NONE',  ( 6.534533895392296010, -5.902695350657468865, 6.631005141235907328E-15 ) ) ;
#3361 = CARTESIAN_POINT ( 'NONE',  ( 43.33558569842703179, 61.09948385550240602, -2.141517661632099223 ) ) ;
#3362 = AXIS2_PLACEMENT_3D ( 'NONE', #2388, #12896, #3046 ) ;
#3363 = LINE ( 'NONE', #2518, #10704 ) ;
#3364 = AXIS2_PLACEMENT_3D ( 'NONE', #7013, #11224, #4879 ) ;
#3365 = ORIENTED_EDGE ( 'NONE', *, *, #7224, .T. ) ;
#3366 = APPLICATION_CONTEXT ( 'automotive_design' ) ;
#3367 = ORIENTED_EDGE ( 'NONE', *, *, #2365, .T. ) ;
#3368 = ORIENTED_EDGE ( 'NONE', *, *, #13564, .T. ) ;
#3369 = CARTESIAN_POINT ( 'NONE',  ( 4.200000000000001954, 0.000000000000000000, 0.000000000000000000 ) ) ;
#3370 = CARTESIAN_POINT ( 'NONE',  ( 0.000000000000000000, -4.330127018922188320, 2.500000000000010214 ) ) ;
#3371 = CARTESIAN_POINT ( 'NONE',  ( -2.171643655288372443, 3.365003104552320767, 2.541098841762897165E-18 ) ) ;
#3372 =( NAMED_UNIT ( * ) SI_UNIT ( $, .STERADIAN. ) SOLID_ANGLE_UNIT ( ) );
#3373 = CARTESIAN_POINT ( 'NONE',  ( 20.00000000000000000, -25.00000000000000711, -23.00000000000000000 ) ) ;
#3374 = CARTESIAN_POINT ( 'NONE',  ( 55.96859303347805081, 52.19948385550240033, 4.306917132069425058 ) ) ;
#3375 = VECTOR ( 'NONE', #5698, 1000.000000000000000 ) ;
#3376 = CARTESIAN_POINT ( 'NONE',  ( 50.02271294988505446, 54.50051614449765935, -7.000000000000000888 ) ) ;
#3377 = CARTESIAN_POINT ( 'NONE',  ( 49.99999999999997158, 45.00000000000001421, -7.499999999999998224 ) ) ;
#3378 = CARTESIAN_POINT ( 'NONE',  ( 50.02271294988512551, 50.49948385550240459, 7.000000000000000888 ) ) ;
#3379 = LINE ( 'NONE', #6373, #6011 ) ;
#3380 = AXIS2_PLACEMENT_3D ( 'NONE', #1306, #6461, #10724 ) ;
#3381 = CARTESIAN_POINT ( 'NONE',  ( 50.02271294988513972, 56.49948385550240459, 8.000000000000001776 ) ) ;
#3382 = EDGE_CURVE ( 'NONE', #11879, #2249, #1167, .T. ) ;
#3383 = ORIENTED_EDGE ( 'NONE', *, *, #3659, .F. ) ;
#3384 = VECTOR ( 'NONE', #8164, 1000.000000000000000 ) ;
#3385 = VERTEX_POINT ( 'NONE', #9480 ) ;
#3386 = DIRECTION ( 'NONE',  ( -0.000000000000000000, -0.000000000000000000, -1.000000000000000000 ) ) ;
#3387 = B_SPLINE_CURVE_WITH_KNOTS ( 'NONE', 3,
 ( #618, #826, #7226, #12533 ),
 .UNSPECIFIED., .F., .F.,
 ( 4, 4 ),
 ( 2.380735200831296902E-07, 0.002921158011986723767 ),
 .UNSPECIFIED. ) ;
#3388 = DIRECTION ( 'NONE',  ( 0.000000000000000000, 0.000000000000000000, 1.000000000000000000 ) ) ;
#3389 = CARTESIAN_POINT ( 'NONE',  ( 44.88205777487401349, 57.80051614449766362, 3.688883143319584779 ) ) ;
#3390 = PLANE ( 'NONE',  #10370 ) ;
#3391 = EDGE_CURVE ( 'NONE', #9340, #13026, #8015, .T. ) ;
#3392 = CARTESIAN_POINT ( 'NONE',  ( 54.72065718078918906, 62.70051614449766220, -6.458785618021089192 ) ) ;
#3393 = DIRECTION ( 'NONE',  ( 0.000000000000000000, 0.000000000000000000, 1.000000000000000000 ) ) ;
#3394 = EDGE_CURVE ( 'NONE', #10160, #4300, #8451, .T. ) ;
#3395 = CARTESIAN_POINT ( 'NONE',  ( 56.79116909180259398, 57.20051614449766220, 4.963592699178938972 ) ) ;
#3396 = ADVANCED_FACE ( 'NONE', ( #5414 ), #10779, .F. ) ;
#3397 = ORIENTED_EDGE ( 'NONE', *, *, #10169, .T. ) ;
#3398 = EDGE_LOOP ( 'NONE', ( #13656, #2279, #115, #3907 ) ) ;
#3399 = EDGE_LOOP ( 'NONE', ( #280, #2770 ) ) ;
#3400 = ORIENTED_EDGE ( 'NONE', *, *, #5195, .T. ) ;
#3401 = CARTESIAN_POINT ( 'NONE',  ( 75.00000000000001421, -7.499999999999971578, -20.00000000000000000 ) ) ;
#3403 = VECTOR ( 'NONE', #1597, 1000.000000000000000 ) ;
#3402 = SURFACE_STYLE_USAGE ( .BOTH. , #1444 ) ;
#3404 = DIRECTION ( 'NONE',  ( -1.000000000000000000, -0.000000000000000000, -0.000000000000000000 ) ) ;
#3405 = CARTESIAN_POINT ( 'NONE',  ( 1.317756351988342622, -3.857995168970215438, -0.04852650426602527628 ) ) ;
#3406 = CARTESIAN_POINT ( 'NONE',  ( 48.07319477248768180, 52.59948385550240602, 6.007379884777225953 ) ) ;
#3407 = CARTESIAN_POINT ( 'NONE',  ( 56.66441430157294690, 44.90051614449765793, -2.141517661632166281 ) ) ;
#3408 = CIRCLE ( 'NONE', #7837, 5.000000000000007994 ) ;
#3409 = CARTESIAN_POINT ( 'NONE',  ( 42.39856655714564226, 48.10051614449766078, -2.493737253992044156 ) ) ;
#3410 = CYLINDRICAL_SURFACE ( 'NONE', #462, 2.649999999999988365 ) ;
#3411 = CARTESIAN_POINT ( 'NONE',  ( 6.367873360227558344, 5.773502691896261751, 0.000000000000000000 ) ) ;
#3412 = CIRCLE ( 'NONE', #9382, 7.500000000000000888 ) ;
#3413 = CARTESIAN_POINT ( 'NONE',  ( 56.65037692655921120, 55.10051614449766078, 2.184720259617097593 ) ) ;
#3414 = CARTESIAN_POINT ( 'NONE',  ( 44.88205777487398507, 63.19948385550240744, -3.688883143319540814 ) ) ;
#3415 = CONICAL_SURFACE ( 'NONE', #3425, 4.000000000000000000, 0.8911886515913786111 ) ;
#3416 = VERTEX_POINT ( 'NONE', #141 ) ;
#3417 = FACE_OUTER_BOUND ( 'NONE', #709, .T. ) ;
#3418 = CIRCLE ( 'NONE', #2757, 2.649999999999988365 ) ;
#3419 = EDGE_LOOP ( 'NONE', ( #7619, #8388, #6978, #10492 ) ) ;
#3420 = CARTESIAN_POINT ( 'NONE',  ( 7.336184427528458230, 0.000000000000000000, 0.000000000000000000 ) ) ;
#3421 = CARTESIAN_POINT ( 'NONE',  ( 50.00000000000000000, 15.00000000000000000, -4.000000000000003553 ) ) ;
#3422 = FACE_OUTER_BOUND ( 'NONE', #8151, .T. ) ;
#3423 = SURFACE_STYLE_FILL_AREA ( #8683 ) ;
#3424 = CARTESIAN_POINT ( 'NONE',  ( 47.74827507625478518, 52.59948385550239180, 7.007379884777227730 ) ) ;
#3425 = AXIS2_PLACEMENT_3D ( 'NONE', #7258, #6096, #7330 ) ;
#3426 = CARTESIAN_POINT ( 'NONE',  ( 3.511755186886750923, -2.826662030176382956, -3.597382984111582083 ) ) ;
#3427 = CARTESIAN_POINT ( 'NONE',  ( 55.69932041026405045, 55.10051614449765367, 1.875703265242156359 ) ) ;
#3428 = DIRECTION ( 'NONE',  ( -1.000000000000000000, 0.000000000000000000, 0.000000000000000000 ) ) ;
#3429 = LINE ( 'NONE', #7652, #12341 ) ;
#3430 = EDGE_CURVE ( 'NONE', #1895, #4695, #13136, .T. ) ;
#3431 = DIRECTION ( 'NONE',  ( -1.000000000000000000, 0.000000000000000000, 0.000000000000000000 ) ) ;
#3432 = CARTESIAN_POINT ( 'NONE',  ( 45.86712807150323812, 57.29948385550240175, -5.649768623646098220 ) ) ;
#3433 = CARTESIAN_POINT ( 'NONE',  ( 0.4465819873852049926, -5.773502691896263528, -3.127607256515468906E-17 ) ) ;
#3434 = VERTEX_POINT ( 'NONE', #9821 ) ;
#3435 = UNCERTAINTY_MEASURE_WITH_UNIT (LENGTH_MEASURE( 1.000000000000000082E-05 ), #886, 'distance_accuracy_value', 'NONE');
#3436 = ORIENTED_EDGE ( 'NONE', *, *, #10318, .T. ) ;
#3437 = CARTESIAN_POINT ( 'NONE',  ( 6.367873360227555679, -2.886751345948119774, 4.999999999999999112 ) ) ;
#3438 = CARTESIAN_POINT ( 'NONE',  ( 0.6920835326022565237, 4.454600218803884459, -3.597382984111579862 ) ) ;
#3439 = CARTESIAN_POINT ( 'NONE',  ( 4.050880675075948290, -1.379097446046192665, -3.567934390854430315 ) ) ;
#3440 =( NAMED_UNIT ( * ) PLANE_ANGLE_UNIT ( ) SI_UNIT ( $, .RADIAN. ) );
#3441 = FACE_OUTER_BOUND ( 'NONE', #2818, .T. ) ;
#3442 = CARTESIAN_POINT ( 'NONE',  ( 49.99999999999997158, 65.00000000000002842, -7.000000000000000888 ) ) ;
#3443 = CARTESIAN_POINT ( 'NONE',  ( 52.29715082351547295, 50.39948385550241028, 6.992620115222774047 ) ) ;
#3444 = CARTESIAN_POINT ( 'NONE',  ( 56.66441430157294690, 56.90051614449766504, -2.141517661632166281 ) ) ;
#3445 = CARTESIAN_POINT ( 'NONE',  ( 0.000000000000000000, 0.000000000000000000, 0.000000000000000000 ) ) ;
#3446 = CARTESIAN_POINT ( 'NONE',  ( 47.70284917648453415, 49.39948385550238896, -6.992620115222774047 ) ) ;
#3447 = LINE ( 'NONE', #5330, #35 ) ;
#3448 = CARTESIAN_POINT ( 'NONE',  ( 58.41169779390614281, 61.99948385550241170, -0.02388180880523160798 ) ) ;
#3449 = EDGE_LOOP ( 'NONE', ( #988, #12456 ) ) ;
#3450 = ORIENTED_EDGE ( 'NONE', *, *, #4766, .F. ) ;
#3451 = ORIENTED_EDGE ( 'NONE', *, *, #10943, .F. ) ;
#3452 = DIRECTION ( 'NONE',  ( -0.000000000000000000, -0.000000000000000000, 1.000000000000000000 ) ) ;
#3453 = VECTOR ( 'NONE', #7233, 1000.000000000000000 ) ;
#3454 = EDGE_CURVE ( 'NONE', #13259, #408, #2690, .T. ) ;
#3455 = CARTESIAN_POINT ( 'NONE',  ( -6.165086708099547508, -6.325508935188330462, 0.000000000000000000 ) ) ;
#3456 = AXIS2_PLACEMENT_3D ( 'NONE', #10931, #3337, #6530 ) ;
#3457 = CARTESIAN_POINT ( 'NONE',  ( 44.30067958973594955, 52.10051614449766788, -1.875703265242155693 ) ) ;
#3458 = CARTESIAN_POINT ( 'NONE',  ( -1.000000000000000000, -14.00000000000000000, 8.999999999999998224 ) ) ;
#3459 = EDGE_CURVE ( 'NONE', #594, #9340, #3800, .T. ) ;
#3460 = CARTESIAN_POINT ( 'NONE',  ( 57.60143344285433642, 49.89948385550241028, -2.493737253992118319 ) ) ;
#3461 = CARTESIAN_POINT ( 'NONE',  ( 42.63976443033212860, 56.99948385550241170, 0.02388180880522514787 ) ) ;
#3462 = CARTESIAN_POINT ( 'NONE',  ( 3.129923130707922496, -23.63917314727666152, -8.999999999999996447 ) ) ;
#3463 = CARTESIAN_POINT ( 'NONE',  ( 42.39856655714564226, 60.10051614449766788, -2.493737253992044156 ) ) ;
#3464 = PRODUCT ( 'idle roller', 'idle roller', '', ( #13419 ) ) ;
#3465 = ORIENTED_EDGE ( 'NONE', *, *, #11081, .T. ) ;
#3466 = EDGE_LOOP ( 'NONE', ( #12772, #3532, #11763 ) ) ;
#3467 = ORIENTED_EDGE ( 'NONE', *, *, #12766, .T. ) ;
#3468 = ORIENTED_EDGE ( 'NONE', *, *, #10740, .T. ) ;
#3469 = CARTESIAN_POINT ( 'NONE',  ( -65.14999999999996305, 32.50000000000001421, 15.00000000000000000 ) ) ;
#3470 = LINE ( 'NONE', #7762, #1930 ) ;
#3471 = DIRECTION ( 'NONE',  ( 1.000000000000000000, 0.000000000000000000, 0.000000000000000000 ) ) ;
#3472 = CARTESIAN_POINT ( 'NONE',  ( 0.000000000000000000, 0.000000000000000000, 5.000000000000000000 ) ) ;
#3473 = DIRECTION ( 'NONE',  ( 0.000000000000000000, 0.000000000000000000, 1.000000000000000000 ) ) ;
#3474 = CARTESIAN_POINT ( 'NONE',  ( 46.45491332379572924, 55.29948385550240175, -4.840751629271157874 ) ) ;
#3475 = CARTESIAN_POINT ( 'NONE',  ( 55.94051828345054389, 45.20051614449765509, 4.345558710429044957 ) ) ;
#3476 = CARTESIAN_POINT ( 'NONE',  ( 54.68390685589039890, 55.30051614449765651, 6.485486291978072693 ) ) ;
#3477 = LINE ( 'NONE', #4444, #5569 ) ;
#3478 = DIRECTION ( 'NONE',  ( -0.5000000000000016653, 0.8660254037844378194, 0.000000000000000000 ) ) ;
#3479 = EDGE_CURVE ( 'NONE', #10164, #7327, #2943, .T. ) ;
#3480 = CARTESIAN_POINT ( 'NONE',  ( 44.05948171654945611, 60.20051614449764799, -4.345558710429044069 ) ) ;
#3481 = ORIENTED_EDGE ( 'NONE', *, *, #10596, .F. ) ;
#3482 = DIRECTION ( 'NONE',  ( -1.000000000000000000, -0.000000000000000000, -0.000000000000000000 ) ) ;
#3483 = ORIENTED_EDGE ( 'NONE', *, *, #3985, .T. ) ;
#3484 = CARTESIAN_POINT ( 'NONE',  ( -3.510273485745307287, -2.827716139362669967, -3.610536846335890004 ) ) ;
#3485 = DIRECTION ( 'NONE',  ( 1.000000000000000000, 0.000000000000000000, 0.000000000000000000 ) ) ;
#3486 = DIRECTION ( 'NONE',  ( 0.000000000000000000, 0.000000000000000000, 1.000000000000000000 ) ) ;
#3487 = EDGE_CURVE ( 'NONE', #6427, #4186, #763, .T. ) ;
#3488 = ADVANCED_FACE ( 'NONE', ( #5819 ), #12036, .F. ) ;
#3489 = CARTESIAN_POINT ( 'NONE',  ( 49.97728705011488159, 59.49948385550240459, -7.000000000000000888 ) ) ;
#3490 = CIRCLE ( 'NONE', #5926, 12.50000000000000000 ) ;
#3491 = DIRECTION ( 'NONE',  ( -1.545477659731174253E-22, 3.805888647522192075E-23, -1.000000000000000000 ) ) ;
#3492 = CARTESIAN_POINT ( 'NONE',  ( 55.69932041026405045, 59.10051614449766078, 1.875703265242156359 ) ) ;
#3493 = CARTESIAN_POINT ( 'NONE',  ( 0.000000000000000000, 0.000000000000000000, -4.000000000000000000 ) ) ;
#3494 = CARTESIAN_POINT ( 'NONE',  ( 4.000000000000000000, 0.000000000000000000, 0.000000000000000000 ) ) ;
#3495 = CARTESIAN_POINT ( 'NONE',  ( 44.30067958973596376, 46.89948385550240317, 1.875703265242204099 ) ) ;
#3496 = CARTESIAN_POINT ( 'NONE',  ( 4.154306624731035846, -2.398490048085128556, -3.721999068284417955 ) ) ;
#3497 = ORIENTED_EDGE ( 'NONE', *, *, #1323, .T. ) ;
#3498 = VERTEX_POINT ( 'NONE', #402 ) ;
#3499 = AXIS2_PLACEMENT_3D ( 'NONE', #442, #8962, #569 ) ;
#3500 = ORIENTED_EDGE ( 'NONE', *, *, #13206, .F. ) ;
#3501 = FACE_BOUND ( 'NONE', #10771, .T. ) ;
#3502 = CIRCLE ( 'NONE', #11460, 5.000000000000000888 ) ;
#3503 = DIRECTION ( 'NONE',  ( -0.000000000000000000, 0.000000000000000000, -1.000000000000000000 ) ) ;
#3504 = DIRECTION ( 'NONE',  ( -0.000000000000000000, 0.000000000000000000, 1.000000000000000000 ) ) ;
#3505 = EDGE_CURVE ( 'NONE', #1915, #11896, #8250, .T. ) ;
#3506 =( LENGTH_UNIT ( ) NAMED_UNIT ( * ) SI_UNIT ( .MILLI., .METRE. ) );
#3507 = FACE_OUTER_BOUND ( 'NONE', #5479, .T. ) ;
#3508 = CYLINDRICAL_SURFACE ( 'NONE', #256, 12.49999999999999645 ) ;
#3509 = CARTESIAN_POINT ( 'NONE',  ( 45.86712807150323812, 53.29948385550240886, -5.649768623646098220 ) ) ;
#3510 = CARTESIAN_POINT ( 'NONE',  ( 56.65037692655921120, 53.10051614449766078, 2.184720259617097593 ) ) ;
#3511 = AXIS2_PLACEMENT_3D ( 'NONE', #2304, #11648, #7315 ) ;
#3512 = DIRECTION ( 'NONE',  ( -0.9995235871707960351, -0.03086419753086420970, 0.000000000000000000 ) ) ;
#3513 = CARTESIAN_POINT ( 'NONE',  ( 45.86712807150323812, 51.29948385550240175, -5.649768623646098220 ) ) ;
#3514 = AXIS2_PLACEMENT_3D ( 'NONE', #1747, #7986, #8198 ) ;
#3515 = CARTESIAN_POINT ( 'NONE',  ( 50.02271294988512551, 48.49948385550240459, 7.000000000000000888 ) ) ;
#3516 = CARTESIAN_POINT ( 'NONE',  ( 47.37792948025162332, 61.39948385550240317, -7.992620115222770494 ) ) ;
#3517 = EDGE_LOOP ( 'NONE', ( #5686, #6143 ) ) ;
#3518 = ORIENTED_EDGE ( 'NONE', *, *, #2975, .T. ) ;
#3519 = PRESENTATION_LAYER_ASSIGNMENT (  '', '', ( #9269 ) ) ;
#3520 = DIRECTION ( 'NONE',  ( -0.000000000000000000, -0.000000000000000000, -1.000000000000000000 ) ) ;
#3521 = ORIENTED_EDGE ( 'NONE', *, *, #2151, .T. ) ;
#3522 = CARTESIAN_POINT ( 'NONE',  ( 5.599999999999999645, 4.041451884327382338, 0.000000000000000000 ) ) ;
#3523 = DIRECTION ( 'NONE',  ( -1.000000000000000000, -0.000000000000000000, -0.000000000000000000 ) ) ;
#3524 = CARTESIAN_POINT ( 'NONE',  ( 44.28664221472221385, 55.90051614449766504, 1.832500667257213722 ) ) ;
#3525 = CARTESIAN_POINT ( 'NONE',  ( 44.05948171654945611, 64.20051614449766930, -4.345558710429044069 ) ) ;
#3526 = PRODUCT_DEFINITION_FORMATION_WITH_SPECIFIED_SOURCE ( 'ANY', '', #11047, .NOT_KNOWN. ) ;
#3527 = CARTESIAN_POINT ( 'NONE',  ( 50.02271294988513972, 54.49948385550240459, 8.000000000000001776 ) ) ;
#3528 = CIRCLE ( 'NONE', #9706, 4.799999999999999822 ) ;
#3529 = CARTESIAN_POINT ( 'NONE',  ( 57.36023556966787851, 53.99948385550239038, -0.02388180880522424582 ) ) ;
#3530 = FACE_OUTER_BOUND ( 'NONE', #8948, .T. ) ;
#3531 = CARTESIAN_POINT ( 'NONE',  ( 43.20883090819742023, 60.20051614449766220, -4.963592699178938972 ) ) ;
#3532 = ORIENTED_EDGE ( 'NONE', *, *, #4472, .F. ) ;
#3533 = ORIENTED_EDGE ( 'NONE', *, *, #6620, .F. ) ;
#3534 = ORIENTED_EDGE ( 'NONE', *, *, #9097, .F. ) ;
#3535 = EDGE_LOOP ( 'NONE', ( #6737, #5076, #12595, #2320 ) ) ;
#3536 = DIRECTION ( 'NONE',  ( -0.000000000000000000, -0.000000000000000000, -1.000000000000000000 ) ) ;
#3537 = VECTOR ( 'NONE', #4369, 1000.000000000000000 ) ;
#3538 = AXIS2_PLACEMENT_3D ( 'NONE', #11242, #12349, #715 ) ;
#3539 = CARTESIAN_POINT ( 'NONE',  ( -75.00000000000001421, 4.999999999999974243, 0.000000000000000000 ) ) ;
#3540 = FILL_AREA_STYLE ('',( #12796 ) ) ;
#3541 = CARTESIAN_POINT ( 'NONE',  ( 55.71335778527780747, 58.09948385550241312, 1.832500667257165983 ) ) ;
#3542 = CARTESIAN_POINT ( 'NONE',  ( 45.86712807150329496, 49.70051614449766220, 5.649768623646139964 ) ) ;
#3543 = CARTESIAN_POINT ( 'NONE',  ( 43.18075615816994173, 55.80051614449766362, 4.924951120819380357 ) ) ;
#3544 = APPLICATION_CONTEXT ( 'automotive_design' ) ;
#3545 = CARTESIAN_POINT ( 'NONE',  ( 0.000000000000000000, 0.000000000000000000, -4.000000000000000000 ) ) ;
#3546 = DIRECTION ( 'NONE',  ( -1.000000000000000000, -3.469446951953615175E-16, -0.000000000000000000 ) ) ;
#3547 = CARTESIAN_POINT ( 'NONE',  ( 55.94051828345053679, 63.20051614449765509, 4.345558710429044069 ) ) ;
#3548 = CIRCLE ( 'NONE', #3761, 2.649999999999985700 ) ;
#3549 = ORIENTED_EDGE ( 'NONE', *, *, #4404, .F. ) ;
#3550 = CARTESIAN_POINT ( 'NONE',  ( -3.974344831685191280E-13, 4.796734841935104576, -3.721909803043223608 ) ) ;
#3551 = EDGE_CURVE ( 'NONE', #6051, #844, #4578, .T. ) ;
#3552 = EDGE_LOOP ( 'NONE', ( #12358, #539, #8027, #4846 ) ) ;
#3553 = CARTESIAN_POINT ( 'NONE',  ( 6.367873360227556567, 2.886751345948125991, 4.999999999999999112 ) ) ;
#3554 = DIRECTION ( 'NONE',  ( -1.000000000000000000, 0.000000000000000000, 1.224646799147353207E-16 ) ) ;
#3555 = LINE ( 'NONE', #1389, #1780 ) ;
#3556 = VECTOR ( 'NONE', #9975, 1000.000000000000000 ) ;
#3557 = CARTESIAN_POINT ( 'NONE',  ( 0.000000000000000000, 0.000000000000000000, 0.000000000000000000 ) ) ;
#3558 = CARTESIAN_POINT ( 'NONE',  ( 49.97728705011488159, 57.49948385550241170, -7.000000000000000888 ) ) ;
#3559 = CARTESIAN_POINT ( 'NONE',  ( 46.45491332379576477, 57.70051614449766930, 4.840751629271188961 ) ) ;
#3560 = EDGE_CURVE ( 'NONE', #9611, #13146, #1499, .T. ) ;
#3561 = DIRECTION ( 'NONE',  ( -1.000000000000000000, -0.000000000000000000, -0.000000000000000000 ) ) ;
#3562 = LINE ( 'NONE', #3633, #12990 ) ;
#3563 = EDGE_CURVE ( 'NONE', #10405, #5442, #4049, .T. ) ;
#3564 = CARTESIAN_POINT ( 'NONE',  ( 46.49166364869456913, 62.30051614449766362, -4.867452303228181343 ) ) ;
#3565 = CARTESIAN_POINT ( 'NONE',  ( 45.86712807150323812, 63.29948385550240886, -5.649768623646098220 ) ) ;
#3566 = DIRECTION ( 'NONE',  ( -9.251858538542972814E-17, -1.000000000000000000, 0.000000000000000000 ) ) ;
#3567 = ADVANCED_FACE ( 'NONE', ( #1642, #5885, #1432 ), #10085, .F. ) ;
#3568 = ORIENTED_EDGE ( 'NONE', *, *, #10310, .T. ) ;
#3569 = ORIENTED_EDGE ( 'NONE', *, *, #9506, .F. ) ;
#3570 = VECTOR ( 'NONE', #13562, 1000.000000000000000 ) ;
#3571 = ADVANCED_FACE ( 'NONE', ( #3530 ), #1366, .F. ) ;
#3572 = COLOUR_RGB ( '',1.000000000000000000, 0.9490196078431372140, 0.9098039215686274384 ) ;
#3573 = EDGE_LOOP ( 'NONE', ( #10694, #10646, #10741, #7536, #4165 ) ) ;
#3574 = DIRECTION ( 'NONE',  ( -0.000000000000000000, -0.000000000000000000, 1.000000000000000000 ) ) ;
#3575 = CARTESIAN_POINT ( 'NONE',  ( -0.1750025118121544265, -4.719839900820635314, -3.469254087858253399 ) ) ;
#3576 = CARTESIAN_POINT ( 'NONE',  ( -2.059999999999998721, 2.522772406243545965E-16, -0.3080913168122742518 ) ) ;
#3577 = LINE ( 'NONE', #7866, #5778 ) ;
#3578 = CARTESIAN_POINT ( 'NONE',  ( 4.151274195509685683, -2.039912954708743786, 3.533232880573501156 ) ) ;
#3579 = AXIS2_PLACEMENT_3D ( 'NONE', #9347, #11486, #8766 ) ;
#3580 = CARTESIAN_POINT ( 'NONE',  ( 56.66441430157294690, 50.90051614449766504, -2.141517661632166281 ) ) ;
#3581 = PLANE ( 'NONE',  #9925 ) ;
#3582 = VECTOR ( 'NONE', #7232, 1000.000000000000000 ) ;
#3583 = CARTESIAN_POINT ( 'NONE',  ( 54.09612160359786515, 53.69948385550240744, -5.676469297603166098 ) ) ;
#3584 = CARTESIAN_POINT ( 'NONE',  ( 45.27934281921075410, 65.29948385550241596, -6.458785618021043895 ) ) ;
#3585 = EDGE_CURVE ( 'NONE', #6619, #9887, #8785, .T. ) ;
#3586 = VERTEX_POINT ( 'NONE', #7821 ) ;
#3587 = ORIENTED_EDGE ( 'NONE', *, *, #5113, .F. ) ;
#3588 = CARTESIAN_POINT ( 'NONE',  ( 1.000000000000002442, -20.00000000000000000, 8.999999999999998224 ) ) ;
#3589 = AXIS2_PLACEMENT_3D ( 'NONE', #9032, #13231, #3776 ) ;
#3590 = ORIENTED_EDGE ( 'NONE', *, *, #1777, .F. ) ;
#3591 = CARTESIAN_POINT ( 'NONE',  ( 0.000000000000000000, -3.031088913245534755, -1.750000000000001332 ) ) ;
#3592 = CIRCLE ( 'NONE', #276, 1.500000000000000222 ) ;
#3593 = CARTESIAN_POINT ( 'NONE',  ( 7.336184427528458230, 0.000000000000000000, -8.105212085995399107 ) ) ;
#3594 = CARTESIAN_POINT ( 'NONE',  ( 55.69932041026405045, 57.10051614449766788, 1.875703265242156359 ) ) ;
#3595 = CARTESIAN_POINT ( 'NONE',  ( 0.2174200650117580902, -3.876582599186216616, -0.2855619784720681564 ) ) ;
#3596 = CARTESIAN_POINT ( 'NONE',  ( 41.58830220609386430, 54.99948385550239749, 0.02388180880523263147 ) ) ;
#3597 = CARTESIAN_POINT ( 'NONE',  ( 47.70284917648453415, 59.39948385550241028, -6.992620115222774047 ) ) ;
#3598 = DIRECTION ( 'NONE',  ( 0.000000000000000000, -0.8660254037844380415, 0.5000000000000012212 ) ) ;
#3599 = EDGE_CURVE ( 'NONE', #12887, #7922, #12984, .T. ) ;
#3600 = CARTESIAN_POINT ( 'NONE',  ( 47.42335538002180328, 64.40051614449764372, -8.007379884777206414 ) ) ;
#3601 = AXIS2_PLACEMENT_3D ( 'NONE', #5611, #3598, #6718 ) ;
#3602 = EDGE_CURVE ( 'NONE', #6107, #9574, #6492, .T. ) ;
#3603 = ORIENTED_EDGE ( 'NONE', *, *, #8717, .T. ) ;
#3604 = ORIENTED_EDGE ( 'NONE', *, *, #533, .T. ) ;
#3605 = ORIENTED_EDGE ( 'NONE', *, *, #6787, .T. ) ;
#3606 = ORIENTED_EDGE ( 'NONE', *, *, #5620, .T. ) ;
#3607 = CARTESIAN_POINT ( 'NONE',  ( 6.445127866599365873, 3.194847394660948581, -4.687657648742338701 ) ) ;
#3608 = CLOSED_SHELL ( 'NONE', ( #936, #11073, #4298, #10590, #931, #13593, #163, #11669, #11377, #1839, #2041, #11261, #12385, #12706, #7019, #13489, #7630, #3076, #8981, #3630, #7094, #12062, #264, #10905, #12878, #9841, #1257, #9735, #3832, #10141, #8726, #3069, #11882, #9071, #6213, #7037, #1679, #6700, #9353, #5072 ) ) ;
#3609 = VECTOR ( 'NONE', #11901, 1000.000000000000000 ) ;
#3610 = CARTESIAN_POINT ( 'NONE',  ( 62.49999999999998579, 45.00000000000001421, 15.00000000000000000 ) ) ;
#3611 = DIRECTION ( 'NONE',  ( 1.000000000000000000, -1.734723475976807341E-16, -0.000000000000000000 ) ) ;
#3612 = FACE_OUTER_BOUND ( 'NONE', #1927, .T. ) ;
#3613 = CARTESIAN_POINT ( 'NONE',  ( 0.000000000000000000, 0.000000000000000000, -1.000000000000000000 ) ) ;
#3614 = CARTESIAN_POINT ( 'NONE',  ( 44.91013252490152752, 54.79948385550240175, 3.727524721679198461 ) ) ;
#3615 = DIRECTION ( 'NONE',  ( 9.710251638871371392E-17, 5.969973981896233748E-17, 1.000000000000000000 ) ) ;
#3616 = CARTESIAN_POINT ( 'NONE',  ( 41.58830220609386430, 56.00051614449765935, -0.02388180880514929535 ) ) ;
#3617 = DIRECTION ( 'NONE',  ( -0.000000000000000000, -0.000000000000000000, 1.000000000000000000 ) ) ;
#3618 = DIRECTION ( 'NONE',  ( 0.000000000000000000, 1.000000000000000000, 0.000000000000000000 ) ) ;
#3619 = CARTESIAN_POINT ( 'NONE',  ( 50.02271294988505446, 64.50051614449765225, -7.000000000000000888 ) ) ;
#3620 = ORIENTED_EDGE ( 'NONE', *, *, #3599, .F. ) ;
#3621 = DIRECTION ( 'NONE',  ( 0.000000000000000000, 0.000000000000000000, 1.000000000000000000 ) ) ;
#3622 = AXIS2_PLACEMENT_3D ( 'NONE', #1545, #5865, #570 ) ;
#3623 = VERTEX_POINT ( 'NONE', #8095 ) ;
#3624 = CARTESIAN_POINT ( 'NONE',  ( 0.000000000000000000, 0.000000000000000000, 0.000000000000000000 ) ) ;
#3625 = EDGE_CURVE ( 'NONE', #7328, #9621, #11769, .T. ) ;
#3626 = CARTESIAN_POINT ( 'NONE',  ( 4.180231891692620216, -2.049421325483211653, -3.591231015387276848 ) ) ;
#3627 = DIRECTION ( 'NONE',  ( 1.000000000000000000, 0.000000000000000000, 0.000000000000000000 ) ) ;
#3628 = CARTESIAN_POINT ( 'NONE',  ( 42.63976443033212860, 56.99948385550241170, 0.02388180880522514787 ) ) ;
#3629 = CARTESIAN_POINT ( 'NONE',  ( 53.54508667620424234, 60.70051614449766930, -4.840751629271188961 ) ) ;
#3630 = ADVANCED_FACE ( 'NONE', ( #1134, #1712 ), #12434, .F. ) ;
#3631 = CIRCLE ( 'NONE', #11360, 1.535500000000000087 ) ;
#3632 = DIRECTION ( 'NONE',  ( 0.000000000000000000, 0.000000000000000000, 1.000000000000000000 ) ) ;
#3633 = CARTESIAN_POINT ( 'NONE',  ( 6.080745460913608902, 0.5192545390863916310, -1.000000000000000000 ) ) ;
#3634 = CARTESIAN_POINT ( 'NONE',  ( 46.49166364869456913, 64.30051614449766362, -4.867452303228181343 ) ) ;
#3635 = CARTESIAN_POINT ( 'NONE',  ( 51.97223112728254790, 48.39948385550240317, 5.992620115222778487 ) ) ;
#3636 = DIRECTION ( 'NONE',  ( -0.000000000000000000, 0.000000000000000000, -1.000000000000000000 ) ) ;
#3637 = VERTEX_POINT ( 'NONE', #5958 ) ;
#3638 = AXIS2_PLACEMENT_3D ( 'NONE', #9573, #12736, #7501 ) ;
#3639 = CIRCLE ( 'NONE', #12681, 1.535500000000000087 ) ;
#3640 = VERTEX_POINT ( 'NONE', #9199 ) ;
#3641 = DIRECTION ( 'NONE',  ( 0.000000000000000000, 1.776356839400250465E-15, 1.000000000000000000 ) ) ;
#3642 = AXIS2_PLACEMENT_3D ( 'NONE', #9189, #13452, #12634 ) ;
#3643 = CARTESIAN_POINT ( 'NONE',  ( -12.99038105676654453, -27.50000000000006040, -9.000000000000000000 ) ) ;
#3644 = CARTESIAN_POINT ( 'NONE',  ( -20.00000000000000000, -19.99999999999999289, -20.00000000000000000 ) ) ;
#3645 = CARTESIAN_POINT ( 'NONE',  ( 8.500000000000000000, -5.773502691896263528, 0.000000000000000000 ) ) ;
#3646 = CARTESIAN_POINT ( 'NONE',  ( 2.595115354961440524, -7.673029147243177306, -1.000000000000000000 ) ) ;
#3647 = CARTESIAN_POINT ( 'NONE',  ( 54.13287192849671214, 52.70051614449766220, -5.649768623646139964 ) ) ;
#3648 = CARTESIAN_POINT ( 'NONE',  ( 6.242811304425483598, -0.9953138271174254426, -5.105233480330447549 ) ) ;
#3649 = LINE ( 'NONE', #1765, #4522 ) ;
#3650 = CARTESIAN_POINT ( 'NONE',  ( 54.13287192849676188, 54.29948385550240886, 5.649768623646098220 ) ) ;
#3651 = CARTESIAN_POINT ( 'NONE',  ( 55.94051828345050836, 45.79948385550240886, -4.345558710429104465 ) ) ;
#3652 = CARTESIAN_POINT ( 'NONE',  ( 42.38452918213188525, 61.09948385550241312, -2.450534656007040013 ) ) ;
#3653 = ORIENTED_EDGE ( 'NONE', *, *, #3874, .T. ) ;
#3654 = ORIENTED_EDGE ( 'NONE', *, *, #3284, .T. ) ;
#3655 = FACE_OUTER_BOUND ( 'NONE', #5996, .T. ) ;
#3656 = EDGE_LOOP ( 'NONE', ( #12645, #6036, #4122, #11341 ) ) ;
#3657 = CARTESIAN_POINT ( 'NONE',  ( 1.925929944387235853E-31, 15.00000000000001599, -15.00000000000000000 ) ) ;
#3658 = CYLINDRICAL_SURFACE ( 'NONE', #6835, 1.500000000000000444 ) ;
#3659 = EDGE_CURVE ( 'NONE', #10723, #10160, #66, .T. ) ;
#3660 = CARTESIAN_POINT ( 'NONE',  ( 51.92680522751238925, 57.40051614449767214, 6.007379884777208190 ) ) ;
#3661 = EDGE_CURVE ( 'NONE', #11968, #9204, #7802, .T. ) ;
#3662 = PRODUCT ( 'hex flange bolt small_iso_ISO 4162 - M5 x 40 x 16-N', 'hex flange bolt small_iso_ISO 4162 - M5 x 40 x 16-N', '', ( #8053 ) ) ;
#3663 = CARTESIAN_POINT ( 'NONE',  ( -4.000000000000000000, 2.309401076758498483, -3.433295621305379353 ) ) ;
#3664 = CARTESIAN_POINT ( 'NONE',  ( 54.68390685589033495, 53.69948385550240744, -6.485486291978119766 ) ) ;
#3665 = EDGE_CURVE ( 'NONE', #5544, #4712, #12310, .T. ) ;
#3666 = CARTESIAN_POINT ( 'NONE',  ( 43.34962307344081012, 56.89948385550240317, 2.184720259617164650 ) ) ;
#3667 = DIRECTION ( 'NONE',  ( -9.710251638871371392E-17, -5.969973981896233748E-17, -1.000000000000000000 ) ) ;
#3668 = CARTESIAN_POINT ( 'NONE',  ( 45.27934281921082516, 59.70051614449766220, 6.458785618021089192 ) ) ;
#3669 = ORIENTED_EDGE ( 'NONE', *, *, #8570, .F. ) ;
#3670 = CONTEXT_DEPENDENT_SHAPE_REPRESENTATION ( #6645, #4569 ) ;
#3671 = ORIENTED_EDGE ( 'NONE', *, *, #13281, .T. ) ;
#3672 = AXIS2_PLACEMENT_3D ( 'NONE', #5296, #11371, #2030 ) ;
#3673 = VERTEX_POINT ( 'NONE', #3936 ) ;
#3674 = ORIENTED_EDGE ( 'NONE', *, *, #9986, .T. ) ;
#3675 = DIRECTION ( 'NONE',  ( 1.000000000000000000, -0.000000000000000000, -0.000000000000000000 ) ) ;
#3676 = CARTESIAN_POINT ( 'NONE',  ( 0.000000000000000000, 0.000000000000000000, -0.3080913168122742518 ) ) ;
#3677 = CARTESIAN_POINT ( 'NONE',  ( -74.99999999999998579, -2.602085213965210642E-14, 0.000000000000000000 ) ) ;
#3678 = CARTESIAN_POINT ( 'NONE',  ( 55.11794222512601493, 54.19948385550241454, 3.688883143319541702 ) ) ;
#3679 = CARTESIAN_POINT ( 'NONE',  ( 43.33558569842706021, 45.90051614449765793, 2.141517661632167169 ) ) ;
#3680 = CARTESIAN_POINT ( 'NONE',  ( 45.31609314410960820, 50.30051614449766362, -6.485486291978072693 ) ) ;
#3681 = CARTESIAN_POINT ( 'NONE',  ( 0.000000000000000000, 0.5192545390863916310, -1.000000000000000000 ) ) ;
#3682 = CARTESIAN_POINT ( 'NONE',  ( 0.000000000000000000, 0.000000000000000000, 0.000000000000000000 ) ) ;
#3683 = CARTESIAN_POINT ( 'NONE',  ( 56.65037692655921120, 61.10051614449766078, 2.184720259617097593 ) ) ;
#3684 = EDGE_LOOP ( 'NONE', ( #361, #6347, #3568, #9134, #2607, #8117, #13363, #6671 ) ) ;
#3685 = EDGE_CURVE ( 'NONE', #10142, #12202, #1854, .T. ) ;
#3686 = FACE_OUTER_BOUND ( 'NONE', #9273, .T. ) ;
#3687 = ORIENTED_EDGE ( 'NONE', *, *, #6225, .F. ) ;
#3688 = CARTESIAN_POINT ( 'NONE',  ( -14.14213562373094213, -14.99999999999998757, -23.00000000000000000 ) ) ;
#3689 = CARTESIAN_POINT ( 'NONE',  ( 4.052424581287701777, -3.786734753435149425, -0.5771415817957858962 ) ) ;
#3690 = DIRECTION ( 'NONE',  ( 1.000000000000000000, 0.000000000000000000, 0.000000000000000000 ) ) ;
#3691 = CARTESIAN_POINT ( 'NONE',  ( 43.34962307344081012, 54.89948385550240317, 2.184720259617164650 ) ) ;
#3692 = EDGE_CURVE ( 'NONE', #11894, #13259, #13320, .T. ) ;
#3693 = CARTESIAN_POINT ( 'NONE',  ( 51.97223112728249816, 58.60051614449766788, -5.992620115222793586 ) ) ;
#3694 = CARTESIAN_POINT ( 'NONE',  ( -3.309651814758565180, -5.455921364805393026, 0.000000000000000000 ) ) ;
#3695 = CARTESIAN_POINT ( 'NONE',  ( 6.271006797790669829, 0.9853839345309320930, 5.106080050406710313 ) ) ;
#3696 = CARTESIAN_POINT ( 'NONE',  ( 43.69122665457040000, 62.00051614449766646, -0.02388180880515696977 ) ) ;
#3697 = CARTESIAN_POINT ( 'NONE',  ( 43.69122665457040000, 46.99948385550239749, 0.02388180880521036456 ) ) ;
#3698 = PLANE ( 'NONE',  #9602 ) ;
#3699 = ORIENTED_EDGE ( 'NONE', *, *, #9643, .T. ) ;
#3700 = UNCERTAINTY_MEASURE_WITH_UNIT (LENGTH_MEASURE( 1.000000000000000082E-05 ), #6003, 'distance_accuracy_value', 'NONE');
#3701 = VERTEX_POINT ( 'NONE', #6030 ) ;
#3702 = CARTESIAN_POINT ( 'NONE',  ( 15.00000000000000178, -20.00000000000000000, -23.00000000000000000 ) ) ;
#3703 = AXIS2_PLACEMENT_3D ( 'NONE', #7294, #10526, #9558 ) ;
#3704 = LINE ( 'NONE', #3774, #1419 ) ;
#3705 = CARTESIAN_POINT ( 'NONE',  ( 2.449293598294706513E-15, -20.00000000000000000, 15.00000000000000355 ) ) ;
#3706 = DIRECTION ( 'NONE',  ( 1.000000000000000000, 0.000000000000000000, 0.000000000000000000 ) ) ;
#3707 = DIRECTION ( 'NONE',  ( -0.000000000000000000, 0.000000000000000000, -1.000000000000000000 ) ) ;
#3708 = CARTESIAN_POINT ( 'NONE',  ( 57.36023556966787851, 63.00051614449767357, 0.02388180880515038476 ) ) ;
#3709 = LINE ( 'NONE', #7933, #4206 ) ;
#3710 = CARTESIAN_POINT ( 'NONE',  ( 5.599999999999999645, 0.000000000000000000, 0.000000000000000000 ) ) ;
#3711 = CARTESIAN_POINT ( 'NONE',  ( 47.74827507625478518, 60.59948385550239891, 7.007379884777227730 ) ) ;
#3712 = CARTESIAN_POINT ( 'NONE',  ( 44.05948171654949874, 48.79948385550238754, 4.345558710429105354 ) ) ;
#3713 = CARTESIAN_POINT ( 'NONE',  ( 52.62207051974839089, 62.39948385550240317, 7.992620115222770494 ) ) ;
#3714 = ORIENTED_EDGE ( 'NONE', *, *, #9959, .F. ) ;
#3715 = ORIENTED_EDGE ( 'NONE', *, *, #7033, .T. ) ;
#3716 = CARTESIAN_POINT ( 'NONE',  ( 3.974167765203684866, 0.7238254970431302615, -3.565825589389262085 ) ) ;
#3717 = ORIENTED_EDGE ( 'NONE', *, *, #12089, .T. ) ;
#3718 = CARTESIAN_POINT ( 'NONE',  ( -14.14213562373094213, -14.99999999999998757, -50.00000000000000000 ) ) ;
#3719 = AXIS2_PLACEMENT_3D ( 'NONE', #7726, #5585, #12072 ) ;
#3720 = DIRECTION ( 'NONE',  ( 1.000000000000000000, 0.000000000000000000, 0.000000000000000000 ) ) ;
#3721 = CARTESIAN_POINT ( 'NONE',  ( 53.50833635130544508, 61.30051614449766362, 4.867452303228181343 ) ) ;
#3722 = CARTESIAN_POINT ( 'NONE',  ( 4.000000000000000000, -2.471525695159793035, -3.686886880705770864 ) ) ;
#3723 = CARTESIAN_POINT ( 'NONE',  ( 41.58830220609386430, 52.99948385550241170, 0.02388180880523263147 ) ) ;
#3724 = CARTESIAN_POINT ( 'NONE',  ( 56.65037692655918988, 55.89948385550240317, -2.184720259617163762 ) ) ;
#3725 = CARTESIAN_POINT ( 'NONE',  ( 4.142654963991854622, -4.070796997468703715, 6.968404583626299416E-17 ) ) ;
#3726 = ADVANCED_FACE ( 'NONE', ( #4989 ), #5386, .F. ) ;
#3727 = CARTESIAN_POINT ( 'NONE',  ( 49.97728705011495265, 63.50051614449765935, 8.000000000000001776 ) ) ;
#3728 = CIRCLE ( 'NONE', #11467, 6.080745460913608902 ) ;
#3729 = EDGE_CURVE ( 'NONE', #9887, #3329, #9592, .T. ) ;
#3730 = VERTEX_POINT ( 'NONE', #114 ) ;
#3731 = ADVANCED_FACE ( 'NONE', ( #8304 ), #878, .T. ) ;
#3732 = CONTEXT_DEPENDENT_SHAPE_REPRESENTATION ( #5491, #8434 ) ;
#3733 = ORIENTED_EDGE ( 'NONE', *, *, #9061, .T. ) ;
#3734 = ADVANCED_FACE ( 'NONE', ( #10226 ), #6244, .F. ) ;
#3735 = ORIENTED_EDGE ( 'NONE', *, *, #8148, .F. ) ;
#3736 = ORIENTED_EDGE ( 'NONE', *, *, #2154, .F. ) ;
#3737 = AXIS2_PLACEMENT_3D ( 'NONE', #8542, #2231, #6539 ) ;
#3738 = LINE ( 'NONE', #8030, #10767 ) ;
#3739 =( NAMED_UNIT ( * ) SI_UNIT ( $, .STERADIAN. ) SOLID_ANGLE_UNIT ( ) );
#3740 = DIRECTION ( 'NONE',  ( -0.000000000000000000, -0.000000000000000000, 1.000000000000000000 ) ) ;
#3741 = DIRECTION ( 'NONE',  ( 0.000000000000000000, 0.000000000000000000, 1.000000000000000000 ) ) ;
#3742 = EDGE_CURVE ( 'NONE', #12223, #407, #10368, .T. ) ;
#3743 = DIRECTION ( 'NONE',  ( 0.000000000000000000, 0.000000000000000000, -1.000000000000000000 ) ) ;
#3744 = CIRCLE ( 'NONE', #13249, 0.2000000000000000944 ) ;
#3745 = CARTESIAN_POINT ( 'NONE',  ( 44.28664221472220675, 55.09948385550241312, -1.832500667257165317 ) ) ;
#3746 = CARTESIAN_POINT ( 'NONE',  ( 49.97728705011495265, 51.50051614449765935, 7.000000000000000888 ) ) ;
#3747 = CARTESIAN_POINT ( 'NONE',  ( 56.81924384183006538, 54.80051614449764941, -4.924951120819380357 ) ) ;
#3748 = CONICAL_SURFACE ( 'NONE', #9494, 1.999999999999998224, 1.029744259999999745 ) ;
#3749 = DIRECTION ( 'NONE',  ( 0.04542589977017006536, -0.9989677110047503472, 0.000000000000000000 ) ) ;
#3750 = FACE_OUTER_BOUND ( 'NONE', #4865, .T. ) ;
#3751 = CARTESIAN_POINT ( 'NONE',  ( 43.18075615816994173, 45.80051614449766362, 4.924951120819380357 ) ) ;
#3752 = ORIENTED_EDGE ( 'NONE', *, *, #8841, .F. ) ;
#3753 = CONICAL_SURFACE ( 'NONE', #8176, 4.000000000000000000, 0.8911886515913786111 ) ;
#3754 = LINE ( 'NONE', #1736, #7736 ) ;
#3755 = EDGE_LOOP ( 'NONE', ( #3082, #10073, #824, #6572, #8824, #1139, #9357, #10974, #1989, #6075, #5455, #8743, #1941, #5042, #12056, #6328, #5172, #1082, #5616, #9808 ) ) ;
#3756 = LINE ( 'NONE', #13147, #12459 ) ;
#3757 = DIRECTION ( 'NONE',  ( -1.000000000000000000, 0.000000000000000000, 0.000000000000000000 ) ) ;
#3758 = DIRECTION ( 'NONE',  ( 0.000000000000000000, 0.000000000000000000, 1.000000000000000000 ) ) ;
#3759 = CARTESIAN_POINT ( 'NONE',  ( 56.65037692655918988, 57.89948385550240317, -2.184720259617163762 ) ) ;
#3760 = CARTESIAN_POINT ( 'NONE',  ( 49.97728705011488159, 49.49948385550240459, -7.000000000000000888 ) ) ;
#3761 = AXIS2_PLACEMENT_3D ( 'NONE', #7833, #4577, #7763 ) ;
#3762 = DIRECTION ( 'NONE',  ( 0.000000000000000000, 0.000000000000000000, 1.000000000000000000 ) ) ;
#3763 = CARTESIAN_POINT ( 'NONE',  ( 6.080745460913608902, 0.5192545390863916310, -1.000000000000000000 ) ) ;
#3764 = DIRECTION ( 'NONE',  ( -1.000000000000000000, 0.000000000000000000, 0.000000000000000000 ) ) ;
#3765 = CARTESIAN_POINT ( 'NONE',  ( 49.97728705011495265, 47.50051614449766646, 7.000000000000000888 ) ) ;
#3766 = CARTESIAN_POINT ( 'NONE',  ( 43.34962307344081012, 64.89948385550239607, 2.184720259617164650 ) ) ;
#3767 = CARTESIAN_POINT ( 'NONE',  ( 2.449293598294706513E-15, -20.00000000000000000, -9.000000000000000000 ) ) ;
#3768 = ORIENTED_EDGE ( 'NONE', *, *, #12355, .T. ) ;
#3769 = EDGE_CURVE ( 'NONE', #1421, #2711, #5056, .T. ) ;
#3770 = VERTEX_POINT ( 'NONE', #4081 ) ;
#3771 = VERTEX_POINT ( 'NONE', #7267 ) ;
#3772 = DIRECTION ( 'NONE',  ( 0.000000000000000000, 0.000000000000000000, 1.000000000000000000 ) ) ;
#3773 = VECTOR ( 'NONE', #9334, 999.9999999999998863 ) ;
#3774 = CARTESIAN_POINT ( 'NONE',  ( -1.498123826657861590, -5.075000000000000178, 0.000000000000000000 ) ) ;
#3775 = CARTESIAN_POINT ( 'NONE',  ( 6.390983399715594260, -5.837459000499769957, 0.1107755759658282380 ) ) ;
#3776 = DIRECTION ( 'NONE',  ( 0.000000000000000000, 0.000000000000000000, -1.000000000000000000 ) ) ;
#3777 = DIRECTION ( 'NONE',  ( 0.000000000000000000, 0.000000000000000000, 1.000000000000000000 ) ) ;
#3778 = CARTESIAN_POINT ( 'NONE',  ( 43.33558569842706021, 59.90051614449766504, 2.141517661632167169 ) ) ;
#3779 = CARTESIAN_POINT ( 'NONE',  ( 3.973110223767137850, -2.261493176400255405E-11, -3.565797985667433334 ) ) ;
#3780 = CARTESIAN_POINT ( 'NONE',  ( 44.28664221472221385, 45.90051614449766504, 1.832500667257213722 ) ) ;
#3781 = DIRECTION ( 'NONE',  ( 1.000000000000000000, 0.000000000000000000, 0.000000000000000000 ) ) ;
#3782 = CARTESIAN_POINT ( 'NONE',  ( 42.63976443033212860, 60.99948385550238328, 0.02388180880522514787 ) ) ;
#3783 = CARTESIAN_POINT ( 'NONE',  ( 49.97728705011488159, 49.49948385550240459, -7.000000000000000888 ) ) ;
#3784 = CIRCLE ( 'NONE', #10841, 0.5155456020628804703 ) ;
#3785 = CARTESIAN_POINT ( 'NONE',  ( 54.09612160359786515, 49.69948385550240744, -5.676469297603166098 ) ) ;
#3786 = ORIENTED_EDGE ( 'NONE', *, *, #9731, .F. ) ;
#3787 = ORIENTED_EDGE ( 'NONE', *, *, #8, .T. ) ;
#3788 = CARTESIAN_POINT ( 'NONE',  ( 3.961545574370306966, 1.423222908132971476, -3.499999999999999556 ) ) ;
#3789 = ORIENTED_EDGE ( 'NONE', *, *, #6654, .F. ) ;
#3790 = FACE_OUTER_BOUND ( 'NONE', #1235, .T. ) ;
#3791 = CIRCLE ( 'NONE', #1346, 3.309499999999999886 ) ;
#3792 = VECTOR ( 'NONE', #11808, 999.9999999999998863 ) ;
#3793 = CIRCLE ( 'NONE', #13491, 5.560781378645573980 ) ;
#3794 = ADVANCED_FACE ( 'NONE', ( #4334 ), #8555, .T. ) ;
#3795 = FACE_OUTER_BOUND ( 'NONE', #10680, .T. ) ;
#3796 = CARTESIAN_POINT ( 'NONE',  ( 46.49166364869456913, 62.30051614449766362, -4.867452303228181343 ) ) ;
#3797 = LINE ( 'NONE', #1707, #4408 ) ;
#3798 = CARTESIAN_POINT ( 'NONE',  ( 50.02271294988513972, 56.49948385550240459, 8.000000000000001776 ) ) ;
#3799 = CARTESIAN_POINT ( 'NONE',  ( 44.03140696652192787, 65.19948385550240744, -4.306917132069425058 ) ) ;
#3800 = LINE ( 'NONE', #2483, #4259 ) ;
#3801 = ADVANCED_FACE ( 'NONE', ( #177 ), #2447, .T. ) ;
#3802 = CARTESIAN_POINT ( 'NONE',  ( 43.18075615816989199, 53.19948385550240744, -4.924951120819313743 ) ) ;
#3803 = AXIS2_PLACEMENT_3D ( 'NONE', #1932, #10826, #1342 ) ;
#3804 = ORIENTED_EDGE ( 'NONE', *, *, #13028, .T. ) ;
#3805 = ORIENTED_EDGE ( 'NONE', *, *, #8150, .F. ) ;
#3806 = APPLICATION_CONTEXT ( 'automotive_design' ) ;
#3807 = VERTEX_POINT ( 'NONE', #9917 ) ;
#3808 = ORIENTED_EDGE ( 'NONE', *, *, #8511, .T. ) ;
#3809 = DIRECTION ( 'NONE',  ( 1.000000000000000000, 0.000000000000000000, 0.000000000000000000 ) ) ;
#3810 = LINE ( 'NONE', #4783, #6585 ) ;
#3811 = EDGE_CURVE ( 'NONE', #13345, #1735, #5259, .T. ) ;
#3812 = DIRECTION ( 'NONE',  ( 0.000000000000000000, 0.000000000000000000, 1.000000000000000000 ) ) ;
#3813 = DIRECTION ( 'NONE',  ( 0.000000000000000000, 0.000000000000000000, 1.000000000000000000 ) ) ;
#3814 = DIRECTION ( 'NONE',  ( 1.000000000000000000, -0.000000000000000000, -0.000000000000000000 ) ) ;
#3815 = CARTESIAN_POINT ( 'NONE',  ( 48.07319477248768180, 64.59948385550241312, 6.007379884777225953 ) ) ;
#3816 = CARTESIAN_POINT ( 'NONE',  ( 55.96859303347802239, 52.80051614449765651, -4.306917132069484566 ) ) ;
#3817 = EDGE_CURVE ( 'NONE', #2789, #757, #8823, .T. ) ;
#3818 = CARTESIAN_POINT ( 'NONE',  ( 43.20883090819742023, 62.20051614449766220, -4.963592699178938972 ) ) ;
#3819 = AXIS2_PLACEMENT_3D ( 'NONE', #8180, #5218, #3884 ) ;
#3820 = EDGE_CURVE ( 'NONE', #2249, #7376, #11793, .T. ) ;
#3821 = FILL_AREA_STYLE_COLOUR ( '', #10419 ) ;
#3822 = CARTESIAN_POINT ( 'NONE',  ( 50.38494826773854385, 45.00000000000002842, -6.500000000000005329 ) ) ;
#3823 = CARTESIAN_POINT ( 'NONE',  ( 50.02271294988505446, 62.50051614449766646, -7.000000000000000888 ) ) ;
#3825 = ORIENTED_EDGE ( 'NONE', *, *, #12932, .F. ) ;
#3824 = ORIENTED_EDGE ( 'NONE', *, *, #5839, .T. ) ;
#3826 = CARTESIAN_POINT ( 'NONE',  ( -1.144235203016679359, -3.958177651039096911, -0.09382832055446428676 ) ) ;
#3827 = ORIENTED_EDGE ( 'NONE', *, *, #6073, .F. ) ;
#3828 = PLANE ( 'NONE',  #8709 ) ;
#3829 = CARTESIAN_POINT ( 'NONE',  ( 4.000000000000003553, 0.000000000000000000, 0.000000000000000000 ) ) ;
#3830 = CARTESIAN_POINT ( 'NONE',  ( 57.36023556966787851, 63.99948385550241881, -0.02388180880522424582 ) ) ;
#3831 = CARTESIAN_POINT ( 'NONE',  ( 45.90387839640214196, 58.69948385550240033, 5.676469297603166098 ) ) ;
#3832 = ADVANCED_FACE ( 'NONE', ( #13023 ), #8691, .F. ) ;
#3833 = DIRECTION ( 'NONE',  ( 1.000000000000000000, 0.000000000000000000, 0.000000000000000000 ) ) ;
#3834 = CARTESIAN_POINT ( 'NONE',  ( -20.00000000000000000, -19.99999999999999289, -23.00000000000000000 ) ) ;
#3835 = CARTESIAN_POINT ( 'NONE',  ( 55.11794222512599362, 62.80051614449766362, -3.688883143319583446 ) ) ;
#3836 = CARTESIAN_POINT ( 'NONE',  ( 51.97223112728254790, 50.39948385550241738, 5.992620115222778487 ) ) ;
#3837 = DIRECTION ( 'NONE',  ( 0.000000000000000000, 0.000000000000000000, -1.000000000000000000 ) ) ;
#3838 = VERTEX_POINT ( 'NONE', #10693 ) ;
#3839 = ORIENTED_EDGE ( 'NONE', *, *, #10737, .T. ) ;
#3840 = EDGE_LOOP ( 'NONE', ( #3714, #580, #4433, #6988 ) ) ;
#3841 = DIRECTION ( 'NONE',  ( 1.000000000000000000, 0.000000000000000000, 0.000000000000000000 ) ) ;
#3842 = DIRECTION ( 'NONE',  ( -1.000000000000000000, 0.000000000000000000, 0.000000000000000000 ) ) ;
#3843 = LINE ( 'NONE', #6963, #4003 ) ;
#3844 = CARTESIAN_POINT ( 'NONE',  ( -3.734041964264191549, -23.01611183630746638, -8.999999999999996447 ) ) ;
#3845 = CARTESIAN_POINT ( 'NONE',  ( -29.99999999999999645, 40.00000000000000000, -9.999999999999998224 ) ) ;
#3846 = AXIS2_PLACEMENT_3D ( 'NONE', #10322, #4871, #3892 ) ;
#3847 = CARTESIAN_POINT ( 'NONE',  ( 56.66441430157294690, 58.90051614449766504, -2.141517661632166281 ) ) ;
#3848 = DIRECTION ( 'NONE',  ( 1.000000000000000000, 0.000000000000000000, 0.000000000000000000 ) ) ;
#3849 = CARTESIAN_POINT ( 'NONE',  ( 56.30877334542961421, 63.99948385550241170, -0.02388180880520959434 ) ) ;
#3850 = CARTESIAN_POINT ( 'NONE',  ( -14.92500000000000249, -18.50187617334218970, 9.000000000000000000 ) ) ;
#3851 = AXIS2_PLACEMENT_3D ( 'NONE', #10404, #917, #5169 ) ;
#3852 = CARTESIAN_POINT ( 'NONE',  ( 52.25172492374522903, 61.59948385550239891, -7.007379884777225953 ) ) ;
#3853 = CARTESIAN_POINT ( 'NONE',  ( 42.63976443033212860, 52.99948385550240459, 0.02388180880522514787 ) ) ;
#3854 = AXIS2_PLACEMENT_3D ( 'NONE', #3048, #5213, #13613 ) ;
#3855 = CARTESIAN_POINT ( 'NONE',  ( 45.86712807150323812, 49.29948385550240175, -5.649768623646098220 ) ) ;
#3856 = AXIS2_PLACEMENT_3D ( 'NONE', #3657, #10077, #2756 ) ;
#3857 = ORIENTED_EDGE ( 'NONE', *, *, #3321, .T. ) ;
#3858 = ORIENTED_EDGE ( 'NONE', *, *, #1435, .T. ) ;
#3859 = DIRECTION ( 'NONE',  ( 0.000000000000000000, 0.000000000000000000, 1.000000000000000000 ) ) ;
#3860 = ORIENTED_EDGE ( 'NONE', *, *, #11926, .T. ) ;
#3861 = FACE_OUTER_BOUND ( 'NONE', #566, .T. ) ;
#3862 = CIRCLE ( 'NONE', #5635, 15.00000000000000000 ) ;
#3863 = CARTESIAN_POINT ( 'NONE',  ( 1.250000000000000000, -6.429618962271402616, -1.000000000000000000 ) ) ;
#3864 = CARTESIAN_POINT ( 'NONE',  ( 55.08986747509849380, 61.20051614449766220, 3.727524721679155384 ) ) ;
#3865 = CARTESIAN_POINT ( 'NONE',  ( 4.000000000000000000, 1.680228229147133767, -3.316631783032546021 ) ) ;
#3866 = CARTESIAN_POINT ( 'NONE',  ( 57.60143344285433642, 59.89948385550240317, -2.493737253992118319 ) ) ;
#3867 = CARTESIAN_POINT ( 'NONE',  ( -30.00000000000000000, 7.499999999999996447, -9.999999999999994671 ) ) ;
#3868 = DIRECTION ( 'NONE',  ( 0.9995235871707960351, -0.03086419753086420970, 0.000000000000000000 ) ) ;
#3869 = CARTESIAN_POINT ( 'NONE',  ( 56.81924384183011512, 48.19948385550240744, 4.924951120819313743 ) ) ;
#3870 = EDGE_LOOP ( 'NONE', ( #12509, #1157, #2363, #210 ) ) ;
#3871 = VERTEX_POINT ( 'NONE', #7518 ) ;
#3872 = B_SPLINE_CURVE_WITH_KNOTS ( 'NONE', 3,
 ( #1884, #6195, #12461, #2790, #8189, #11362, #4107, #4944 ),
 .UNSPECIFIED., .F., .F.,
 ( 4, 2, 2, 4 ),
 ( 0.002921158011986723767, 0.003648658599403076588, 0.004376159186819428976, 0.005831160361652133750 ),
 .UNSPECIFIED. ) ;
#3873 = EDGE_LOOP ( 'NONE', ( #7774, #613, #4627, #375 ) ) ;
#3874 = EDGE_CURVE ( 'NONE', #4365, #6658, #7719, .T. ) ;
#3875 = ORIENTED_EDGE ( 'NONE', *, *, #6349, .T. ) ;
#3876 = CARTESIAN_POINT ( 'NONE',  ( 0.000000000000000000, -4.330127018922193649, -2.500000000000000000 ) ) ;
#3877 = DIRECTION ( 'NONE',  ( -0.000000000000000000, -0.000000000000000000, 1.000000000000000000 ) ) ;
#3878 = CARTESIAN_POINT ( 'NONE',  ( -2.649999999999988365, 15.00000000000001599, 15.00000000000000000 ) ) ;
#3879 = CARTESIAN_POINT ( 'NONE',  ( 62.49999999999998579, 32.50000000000001421, 15.00000000000000000 ) ) ;
#3880 = DIRECTION ( 'NONE',  ( 1.000000000000000000, 0.000000000000000000, 0.000000000000000000 ) ) ;
#3881 = CARTESIAN_POINT ( 'NONE',  ( 53.50833635130540955, 61.69948385550240744, -4.867452303228209765 ) ) ;
#3882 = CARTESIAN_POINT ( 'NONE',  ( 47.70284917648459810, 53.60051614449766078, 6.992620115222797139 ) ) ;
#3883 = CARTESIAN_POINT ( 'NONE',  ( 54.68390685589039890, 59.30051614449766362, 6.485486291978072693 ) ) ;
#3884 = DIRECTION ( 'NONE',  ( 1.000000000000000000, 0.000000000000000000, 0.000000000000000000 ) ) ;
#3885 = CARTESIAN_POINT ( 'NONE',  ( 54.72065718078918906, 50.70051614449766220, -6.458785618021089192 ) ) ;
#3886 = CIRCLE ( 'NONE', #12276, 2.649999999999989697 ) ;
#3888 = ORIENTED_EDGE ( 'NONE', *, *, #2109, .F. ) ;
#3887 = EDGE_LOOP ( 'NONE', ( #8727, #8328, #6236, #96 ) ) ;
#3889 = LINE ( 'NONE', #7077, #9049 ) ;
#3890 = ORIENTED_EDGE ( 'NONE', *, *, #11945, .T. ) ;
#3891 = VERTEX_POINT ( 'NONE', #5717 ) ;
#3892 = DIRECTION ( 'NONE',  ( -1.000000000000000000, 0.000000000000000000, 0.000000000000000000 ) ) ;
#3893 = DIRECTION ( 'NONE',  ( 0.000000000000000000, 0.000000000000000000, -1.000000000000000000 ) ) ;
#3894 = CARTESIAN_POINT ( 'NONE',  ( 50.02271294988512551, 64.49948385550240459, 7.000000000000000888 ) ) ;
#3895 = CARTESIAN_POINT ( 'NONE',  ( 57.36023556966787851, 55.99948385550239749, -0.02388180880522424582 ) ) ;
#3896 = ADVANCED_FACE ( 'NONE', ( #4605 ), #11925, .F. ) ;
#3897 = SHAPE_REPRESENTATION ( 'idle-roller mover', ( #430 ), #10167 ) ;
#3898=STYLED_ITEM('',(#13712),#1187);
#3899 = DIRECTION ( 'NONE',  ( -0.000000000000000000, -0.000000000000000000, 1.000000000000000000 ) ) ;
#3900 = CARTESIAN_POINT ( 'NONE',  ( 2.000000000000000000, -1.329782007511005837, 0.7677500000000023750 ) ) ;
#3901 = CYLINDRICAL_SURFACE ( 'NONE', #5733, 2.149999999999999023 ) ;
#3902 = CARTESIAN_POINT ( 'NONE',  ( 42.63976443033212860, 54.00051614449766646, -0.02388180880514948964 ) ) ;
#3903 = CARTESIAN_POINT ( 'NONE',  ( 56.30877334542961421, 49.99948385550240459, -0.02388180880520959434 ) ) ;
#3904 = FACE_OUTER_BOUND ( 'NONE', #7, .T. ) ;
#3905 = EDGE_LOOP ( 'NONE', ( #4499, #1424, #7220, #10201 ) ) ;
#3906 = VERTEX_POINT ( 'NONE', #12819 ) ;
#3908 = EDGE_CURVE ( 'NONE', #10197, #5875, #3363, .T. ) ;
#3907 = ORIENTED_EDGE ( 'NONE', *, *, #12945, .T. ) ;
#3909 = CARTESIAN_POINT ( 'NONE',  ( 4.175572532730932096, -2.061029303918058275, -3.569807470274390493 ) ) ;
#3910 = ADVANCED_FACE ( 'NONE', ( #10954 ), #7587, .T. ) ;
#3911 = CARTESIAN_POINT ( 'NONE',  ( 6.207671477328021048, 3.321994320370322828, -4.246137054663353005 ) ) ;
#3912 = CARTESIAN_POINT ( 'NONE',  ( 3.098410542199072637, -7.060458129626440815, -1.000000000000000000 ) ) ;
#3913 =( NAMED_UNIT ( * ) PLANE_ANGLE_UNIT ( ) SI_UNIT ( $, .RADIAN. ) );
#3914 = FACE_OUTER_BOUND ( 'NONE', #5671, .T. ) ;
#3915 = CARTESIAN_POINT ( 'NONE',  ( -12.99038105676659427, -12.50000000000003020, -9.000000000000000000 ) ) ;
#3916 = CARTESIAN_POINT ( 'NONE',  ( 50.02271294988506156, 46.50051614449766646, -6.000000000000000888 ) ) ;
#3917 = CARTESIAN_POINT ( 'NONE',  ( -9.999999999999998224, 15.00000000000001776, 9.999999999999998224 ) ) ;
#3918 = CARTESIAN_POINT ( 'NONE',  ( 50.02271294988512551, 56.49948385550240459, 7.000000000000000888 ) ) ;
#3919 = CARTESIAN_POINT ( 'NONE',  ( 47.74827507625478518, 50.59948385550238470, 7.007379884777227730 ) ) ;
#3920 = VERTEX_POINT ( 'NONE', #1470 ) ;
#3921 = CARTESIAN_POINT ( 'NONE',  ( 56.66441430157296821, 48.09948385550240602, 2.141517661632100111 ) ) ;
#3922 = ORIENTED_EDGE ( 'NONE', *, *, #1300, .F. ) ;
#3923 = FACE_OUTER_BOUND ( 'NONE', #6975, .T. ) ;
#3924 = EDGE_CURVE ( 'NONE', #10124, #13345, #5626, .T. ) ;
#3925 = B_SPLINE_CURVE_WITH_KNOTS ( 'NONE', 3,
 ( #6076, #3909, #12410, #12274, #13433, #12340, #2874, #4123, #2947, #2808, #11446, #8135, #13365, #9173, #8067, #9380 ),
 .UNSPECIFIED., .F., .F.,
 ( 4, 3, 3, 3, 3, 4 ),
 ( -2.111273352581287704E-06, 0.000000000000000000, 3.519286887794526448E-05, 7.191842652068348909E-05, 0.0001049868727093649664, 0.0001382836236822123786 ),
 .UNSPECIFIED. ) ;
#3926 = VERTEX_POINT ( 'NONE', #5581 ) ;
#3927 = DIRECTION ( 'NONE',  ( -1.000000000000000000, 0.000000000000000000, 0.000000000000000000 ) ) ;
#3928 = FACE_OUTER_BOUND ( 'NONE', #3237, .T. ) ;
#3929 = FACE_OUTER_BOUND ( 'NONE', #8624, .T. ) ;
#3930 = CARTESIAN_POINT ( 'NONE',  ( 46.45491332379576477, 59.70051614449766220, 4.840751629271188961 ) ) ;
#3931 = VECTOR ( 'NONE', #4575, 1000.000000000000000 ) ;
#3932 = DIRECTION ( 'NONE',  ( 1.000000000000000000, 0.000000000000000000, 0.000000000000000000 ) ) ;
#3933 = EDGE_CURVE ( 'NONE', #6494, #8472, #13323, .T. ) ;
#3934 = CARTESIAN_POINT ( 'NONE',  ( 43.20883090819745576, 60.79948385550241596, 4.963592699179006473 ) ) ;
#3935 = CARTESIAN_POINT ( 'NONE',  ( 55.94051828345050836, 61.79948385550239465, -4.345558710429104465 ) ) ;
#3936 = CARTESIAN_POINT ( 'NONE',  ( 5.000000000000003553, -20.00000000000000000, 9.000000000000000000 ) ) ;
#3937 = CARTESIAN_POINT ( 'NONE',  ( 41.58830220609386430, 50.99948385550241170, 0.02388180880523263147 ) ) ;
#3938 = ORIENTED_EDGE ( 'NONE', *, *, #11678, .F. ) ;
#3939 = VERTEX_POINT ( 'NONE', #2380 ) ;
#3940 = EDGE_LOOP ( 'NONE', ( #1034, #2573, #4866, #344 ) ) ;
#3941 = CIRCLE ( 'NONE', #10564, 4.799999999999999822 ) ;
#3942 = FACE_OUTER_BOUND ( 'NONE', #9610, .T. ) ;
#3943 = CIRCLE ( 'NONE', #7484, 5.000000000000000888 ) ;
#3944 = CARTESIAN_POINT ( 'NONE',  ( 2.449293598294706513E-15, -20.00000000000000000, -8.999999999999998224 ) ) ;
#3945 = DIRECTION ( 'NONE',  ( 1.000000000000000000, 3.469446951953615668E-16, -0.000000000000000000 ) ) ;
#3946 = CARTESIAN_POINT ( 'NONE',  ( 12.17636723815389566, -28.75991329190035373, 9.000000000000000000 ) ) ;
#3947 = CARTESIAN_POINT ( 'NONE',  ( 4.211140560182196957, 2.431303136016536470, -3.745885042887433514 ) ) ;
#3948 = CARTESIAN_POINT ( 'NONE',  ( 55.11794222512601493, 62.19948385550240744, 3.688883143319541702 ) ) ;
#3949 = CARTESIAN_POINT ( 'NONE',  ( 43.33558569842706021, 55.90051614449765793, 2.141517661632167169 ) ) ;
#3950 = CARTESIAN_POINT ( 'NONE',  ( 56.79116909180259398, 59.20051614449766220, 4.963592699178938972 ) ) ;
#3951 = VECTOR ( 'NONE', #7706, 1000.000000000000000 ) ;
#3952 = DIRECTION ( 'NONE',  ( 1.000000000000000000, 0.000000000000000000, 0.000000000000000000 ) ) ;
#3953 = CARTESIAN_POINT ( 'NONE',  ( 47.37792948025170858, 47.60051614449766078, 7.992620115222797139 ) ) ;
#3954 = CIRCLE ( 'NONE', #12776, 15.00000000000000000 ) ;
#3956 = ORIENTED_EDGE ( 'NONE', *, *, #706, .T. ) ;
#3955 = EDGE_LOOP ( 'NONE', ( #3752, #9829, #13189, #13078, #2469 ) ) ;
#3957 = ORIENTED_EDGE ( 'NONE', *, *, #5425, .F. ) ;
#3958 = VERTEX_POINT ( 'NONE', #11725 ) ;
#3959 = ORIENTED_EDGE ( 'NONE', *, *, #7633, .F. ) ;
#3960 = CARTESIAN_POINT ( 'NONE',  ( -75.00000000000001421, -5.000000000000025757, 6.123233995736766282E-16 ) ) ;
#3961 = CARTESIAN_POINT ( 'NONE',  ( 15.00000000000000355, -19.99999999999984368, -9.000000000000000000 ) ) ;
#3962 = APPLICATION_PROTOCOL_DEFINITION ( 'draft international standard', 'automotive_design', 1998, #2836 ) ;
#3963 = CARTESIAN_POINT ( 'NONE',  ( 55.94051828345050836, 61.79948385550239465, -4.345558710429104465 ) ) ;
#3964 = CARTESIAN_POINT ( 'NONE',  ( 57.36023556966787851, 59.99948385550240459, -0.02388180880522424582 ) ) ;
#3965 = CARTESIAN_POINT ( 'NONE',  ( 13.99999999999999822, 0.000000000000000000, 1.610000000000000098 ) ) ;
#3966 = CARTESIAN_POINT ( 'NONE',  ( -8.759913291900394583, -32.17636723815387256, 9.000000000000000000 ) ) ;
#3967 = ORIENTED_EDGE ( 'NONE', *, *, #12275, .F. ) ;
#3968 = DIRECTION ( 'NONE',  ( -1.000000000000000000, 0.000000000000000000, -0.000000000000000000 ) ) ;
#3969 = CARTESIAN_POINT ( 'NONE',  ( 56.66441430157294690, 50.90051614449766504, -2.141517661632166281 ) ) ;
#3970 = CARTESIAN_POINT ( 'NONE',  ( 48.07319477248768180, 50.59948385550240602, 6.007379884777225953 ) ) ;
#3971 = CIRCLE ( 'NONE', #10155, 1.535500000000000087 ) ;
#3972 = DIRECTION ( 'NONE',  ( 1.000000000000000000, -0.000000000000000000, 0.000000000000000000 ) ) ;
#3973 = ADVANCED_FACE ( 'NONE', ( #308 ), #4671, .F. ) ;
#3974 = ORIENTED_EDGE ( 'NONE', *, *, #8638, .T. ) ;
#3975 = CARTESIAN_POINT ( 'NONE',  ( 52.80949999999998568, 4.898587196589412829E-16, -4.000000000000000000 ) ) ;
#3976 = EDGE_LOOP ( 'NONE', ( #4977, #78, #6907, #11306 ) ) ;
#3977 = ORIENTED_EDGE ( 'NONE', *, *, #343, .T. ) ;
#3978 = LINE ( 'NONE', #847, #1502 ) ;
#3979 = CARTESIAN_POINT ( 'NONE',  ( 4.071447262713888016, -2.020725942163694722, -3.499999999999999556 ) ) ;
#3980 = CARTESIAN_POINT ( 'NONE',  ( -0.9999999999999976685, -20.00000000000000000, 8.999999999999998224 ) ) ;
#3981 = AXIS2_PLACEMENT_3D ( 'NONE', #1255, #5448, #2240 ) ;
#3982 = CARTESIAN_POINT ( 'NONE',  ( 52.25172492374522903, 47.59948385550239891, -7.007379884777225953 ) ) ;
#3983 = CARTESIAN_POINT ( 'NONE',  ( -13.67449106481164733, -26.16508670809959725, -9.000000000000000000 ) ) ;
#3984 = EDGE_CURVE ( 'NONE', #4066, #614, #9982, .T. ) ;
#3985 = EDGE_CURVE ( 'NONE', #1302, #4555, #12462, .T. ) ;
#3986 = CARTESIAN_POINT ( 'NONE',  ( -65.14999999999996305, 32.50000000000001421, 9.999999999999998224 ) ) ;
#3987 = CARTESIAN_POINT ( 'NONE',  ( 46.45491332379576477, 45.70051614449766220, 4.840751629271188961 ) ) ;
#3988 = EDGE_CURVE ( 'NONE', #9307, #6035, #1401, .T. ) ;
#3989 = FACE_OUTER_BOUND ( 'NONE', #4848, .T. ) ;
#3990 = CARTESIAN_POINT ( 'NONE',  ( 44.03140696652192787, 59.19948385550238612, -4.306917132069425058 ) ) ;
#3991 = CARTESIAN_POINT ( 'NONE',  ( 43.34962307344081012, 50.89948385550241028, 2.184720259617164650 ) ) ;
#3992 = EDGE_CURVE ( 'NONE', #10837, #6107, #10267, .T. ) ;
#3993 = EDGE_LOOP ( 'NONE', ( #12436, #12510, #4380, #6170 ) ) ;
#3994 = CARTESIAN_POINT ( 'NONE',  ( 52.29715082351547295, 52.39948385550241738, 6.992620115222774047 ) ) ;
#3995 = VECTOR ( 'NONE', #4490, 1000.000000000000000 ) ;
#3996 = B_SPLINE_CURVE_WITH_KNOTS ( 'NONE', 3,
 ( #5508, #3426, #301, #11854, #6608, #3289, #4388, #7714 ),
 .UNSPECIFIED., .F., .F.,
 ( 4, 2, 2, 4 ),
 ( 0.000000000000000000, 0.002450665683189819262, 0.003675998524784728893, 0.004901331366379639391 ),
 .UNSPECIFIED. ) ;
#3997 = ORIENTED_EDGE ( 'NONE', *, *, #12109, .T. ) ;
#3998 = CARTESIAN_POINT ( 'NONE',  ( 75.00000000000000000, 32.50000000000001421, 15.00000000000000000 ) ) ;
#3999 = VERTEX_POINT ( 'NONE', #2730 ) ;
#4000 = CARTESIAN_POINT ( 'NONE',  ( 4.114405500665256454, 2.025575754679711959, 3.508400121684935424 ) ) ;
#4001 = CARTESIAN_POINT ( 'NONE',  ( 2.449293598294706513E-15, -20.00000000000000000, -9.000000000000000000 ) ) ;
#4002 = CARTESIAN_POINT ( 'NONE',  ( 57.36023556966787851, 47.99948385550239749, -0.02388180880522424582 ) ) ;
#4003 = VECTOR ( 'NONE', #11309, 1000.000000000000114 ) ;
#4004 = CARTESIAN_POINT ( 'NONE',  ( 46.45491332379576477, 61.70051614449766220, 4.840751629271188961 ) ) ;
#4005 = PRODUCT ( 'MAS-183', 'MAS-183', '', ( #1390 ) ) ;
#4006 = CARTESIAN_POINT ( 'NONE',  ( -20.00000000000000000, -19.99999999999999289, -20.00000000000000000 ) ) ;
#4007 = CARTESIAN_POINT ( 'NONE',  ( 56.81924384183011512, 62.19948385550240744, 4.924951120819313743 ) ) ;
#4008 = EDGE_CURVE ( 'NONE', #13009, #10020, #6305, .T. ) ;
#4009 = DIRECTION ( 'NONE',  ( -9.710251638871371392E-17, -5.969973981896233748E-17, -1.000000000000000000 ) ) ;
#4010 = CARTESIAN_POINT ( 'NONE',  ( 54.72065718078924590, 52.29948385550240886, 6.458785618021043895 ) ) ;
#4011 = ORIENTED_EDGE ( 'NONE', *, *, #5779, .F. ) ;
#4012 = VECTOR ( 'NONE', #477, 1000.000000000000000 ) ;
#4013 = ORIENTED_EDGE ( 'NONE', *, *, #7273, .F. ) ;
#4014 = ORIENTED_EDGE ( 'NONE', *, *, #5140, .T. ) ;
#4015 = AXIS2_PLACEMENT_3D ( 'NONE', #1522, #10866, #6534 ) ;
#4016 = FACE_OUTER_BOUND ( 'NONE', #7604, .T. ) ;
#4017 =( NAMED_UNIT ( * ) PLANE_ANGLE_UNIT ( ) SI_UNIT ( $, .RADIAN. ) );
#4018 = CARTESIAN_POINT ( 'NONE',  ( 62.50000000000000000, 32.50000000000001421, 15.00000000000000000 ) ) ;
#4019 = CARTESIAN_POINT ( 'NONE',  ( 6.270568613849419215, -4.911887854652846386, -1.704496029161938875 ) ) ;
#4020 = CARTESIAN_POINT ( 'NONE',  ( 0.1999999999999987899, 0.000000000000000000, 0.000000000000000000 ) ) ;
#4021 = CARTESIAN_POINT ( 'NONE',  ( 51.97223112728254790, 64.39948385550239607, 5.992620115222778487 ) ) ;
#4022 = CARTESIAN_POINT ( 'NONE',  ( 54.13287192849671214, 52.70051614449766220, -5.649768623646139964 ) ) ;
#4023 = CARTESIAN_POINT ( 'NONE',  ( 47.37792948025170858, 57.60051614449765367, 7.992620115222797139 ) ) ;
#4024 = EDGE_CURVE ( 'NONE', #1117, #4810, #10475, .T. ) ;
#4025 = CONICAL_SURFACE ( 'NONE', #11746, 1.535500000000000087, 1.047197551196590748 ) ;
#4026 = AXIS2_PLACEMENT_3D ( 'NONE', #11640, #8598, #159 ) ;
#4027 = CARTESIAN_POINT ( 'NONE',  ( -4.204114297095464359, 1.660363174096617156, -3.602136431857887011 ) ) ;
#4028 = CARTESIAN_POINT ( 'NONE',  ( 49.97728705011495265, 51.50051614449765935, 8.000000000000001776 ) ) ;
#4030 = VERTEX_POINT ( 'NONE', #11160 ) ;
#4029 = VERTEX_POINT ( 'NONE', #1823 ) ;
#4031 = ORIENTED_EDGE ( 'NONE', *, *, #2716, .T. ) ;
#4032 = UNCERTAINTY_MEASURE_WITH_UNIT (LENGTH_MEASURE( 1.000000000000000082E-05 ), #7764, 'distance_accuracy_value', 'NONE');
#4033 = EDGE_LOOP ( 'NONE', ( #12118, #10245, #5979, #10985 ) ) ;
#4034 = CARTESIAN_POINT ( 'NONE',  ( 6.518095160331716542, 5.866179305615093043, 1.445124054326800857E-15 ) ) ;
#4035 =( NAMED_UNIT ( * ) SI_UNIT ( $, .STERADIAN. ) SOLID_ANGLE_UNIT ( ) );
#4036 = DIRECTION ( 'NONE',  ( 0.8660254037844450359, -0.4999999999999888423, 0.000000000000000000 ) ) ;
#4037 = CARTESIAN_POINT ( 'NONE',  ( 8.500000000000000000, 2.886751345948123770, -5.000000000000000000 ) ) ;
#4038 = CIRCLE ( 'NONE', #3819, 5.000000000000000888 ) ;
#4039 = SHAPE_DEFINITION_REPRESENTATION ( #6565, #11930 ) ;
#4040 = CARTESIAN_POINT ( 'NONE',  ( 47.74827507625478518, 62.59948385550240602, 7.007379884777227730 ) ) ;
#4041 = CARTESIAN_POINT ( 'NONE',  ( 47.70284917648453415, 59.39948385550241028, -6.992620115222774047 ) ) ;
#4042 = DIRECTION ( 'NONE',  ( 1.000000000000000000, 0.000000000000000000, 0.000000000000000000 ) ) ;
#4043 = CARTESIAN_POINT ( 'NONE',  ( 10.00000000000000000, 15.00000000000001776, 15.00000000000000000 ) ) ;
#4044 = LINE ( 'NONE', #2938, #6896 ) ;
#4045 = CARTESIAN_POINT ( 'NONE',  ( 50.02271294988505446, 48.50051614449765935, -7.000000000000000888 ) ) ;
#4046 = CARTESIAN_POINT ( 'NONE',  ( 53.50833635130540955, 49.69948385550240744, -4.867452303228209765 ) ) ;
#4047 = DIRECTION ( 'NONE',  ( -0.000000000000000000, -0.000000000000000000, -1.000000000000000000 ) ) ;
#4048 = ORIENTED_EDGE ( 'NONE', *, *, #4791, .T. ) ;
#4049 = CIRCLE ( 'NONE', #5821, 5.371010071662833063 ) ;
#4050 = CARTESIAN_POINT ( 'NONE',  ( 8.759913291900311094, -7.823632761846075923, 9.000000000000000000 ) ) ;
#4051 = ORIENTED_EDGE ( 'NONE', *, *, #81, .T. ) ;
#4052 = VERTEX_POINT ( 'NONE', #13293 ) ;
#4053 = DIRECTION ( 'NONE',  ( 0.000000000000000000, 0.000000000000000000, 1.000000000000000000 ) ) ;
#4054 = LINE ( 'NONE', #8279, #4070 ) ;
#4055 = DIRECTION ( 'NONE',  ( 1.000000000000000000, 0.000000000000000000, 0.000000000000000000 ) ) ;
#4056 =( NAMED_UNIT ( * ) PLANE_ANGLE_UNIT ( ) SI_UNIT ( $, .RADIAN. ) );
#4057 = DIRECTION ( 'NONE',  ( -0.000000000000000000, -0.000000000000000000, 1.000000000000000000 ) ) ;
#4058 = EDGE_CURVE ( 'NONE', #9221, #10299, #525, .T. ) ;
#4059 = CARTESIAN_POINT ( 'NONE',  ( 4.071447262713890680, -4.041451884327386779, 0.000000000000000000 ) ) ;
#4060 = CARTESIAN_POINT ( 'NONE',  ( 51.92680522751238925, 47.40051614449765793, 6.007379884777208190 ) ) ;
#4061 = CARTESIAN_POINT ( 'NONE',  ( 2.000000000000000000, 1.773042676681340524, -2.059984127722458425E-15 ) ) ;
#4062 = CARTESIAN_POINT ( 'NONE',  ( 52.29715082351547295, 62.39948385550239607, 6.992620115222774047 ) ) ;
#4063 = CARTESIAN_POINT ( 'NONE',  ( 54.13287192849676188, 50.29948385550240175, 5.649768623646098220 ) ) ;
#4064 = ORIENTED_EDGE ( 'NONE', *, *, #6440, .F. ) ;
#4065 = CARTESIAN_POINT ( 'NONE',  ( 55.96859303347804371, 50.19948385550240744, 4.306917132069425946 ) ) ;
#4066 = VERTEX_POINT ( 'NONE', #5788 ) ;
#4067 =( BOUNDED_SURFACE ( )  B_SPLINE_SURFACE ( 3, 2, ( 
 ( #11562, #2072, #7278 ),
 ( #11489, #5141, #13544 ),
 ( #13470, #3117, #4291 ),
 ( #9279, #420, #1869 ),
 ( #9349, #12650, #8379 ),
 ( #2008, #5066, #1934 ) ),
 .UNSPECIFIED., .F., .F., .F. ) 
 B_SPLINE_SURFACE_WITH_KNOTS ( ( 4, 2, 4 ),
 ( 3, 3 ),
 ( 0.02032853247518126225, 0.02278863295364821212, 0.02524873343211516200 ),
 ( 0.000000000000000000, 1.000000000000000000 ),
 .UNSPECIFIED. ) 
 GEOMETRIC_REPRESENTATION_ITEM ( )  RATIONAL_B_SPLINE_SURFACE ( (
 ( 1.000000000000000000, 0.8047781615896835161, 1.000000000000000000),
 ( 1.000000000000000000, 0.8123767586291043008, 1.000000000000000000),
 ( 1.000000000000000000, 0.8190662415562011134, 1.000000000000000000),
 ( 1.000000000000000000, 0.8192361015671398849, 1.000000000000000000),
 ( 1.000000000000000000, 0.8126135807102121689, 1.000000000000000000),
 ( 1.000000000000000000, 0.8047712338318585568, 1.000000000000000000) ) ) 
 REPRESENTATION_ITEM ( '' )  SURFACE ( )  );
#4068 = CARTESIAN_POINT ( 'NONE',  ( 4.052432342741587590, 1.393590342655181891, 3.567979436357439305 ) ) ;
#4069 = ORIENTED_EDGE ( 'NONE', *, *, #1693, .T. ) ;
#4070 = VECTOR ( 'NONE', #9174, 1000.000000000000000 ) ;
#4071 = CARTESIAN_POINT ( 'NONE',  ( 12.99038105676665289, -27.49999999999988276, 9.000000000000000000 ) ) ;
#4072 = CARTESIAN_POINT ( 'NONE',  ( -5.999999999999922728, -32.99038105676662269, -9.000000000000000000 ) ) ;
#4073 = CARTESIAN_POINT ( 'NONE',  ( 43.33558569842703179, 49.09948385550240602, -2.141517661632099223 ) ) ;
#4074 = CIRCLE ( 'NONE', #6086, 2.649999999999988365 ) ;
#4075 =( REPRESENTATION_RELATIONSHIP ('NONE','NONE', #5328, #9196 ) REPRESENTATION_RELATIONSHIP_WITH_TRANSFORMATION ( #2621 )SHAPE_REPRESENTATION_RELATIONSHIP( ) );
#4076 = CARTESIAN_POINT ( 'NONE',  ( 50.02271294988505446, 48.50051614449765935, -7.000000000000000888 ) ) ;
#4077 = PLANE ( 'NONE',  #8844 ) ;
#4078 = CARTESIAN_POINT ( 'NONE',  ( 54.72065718078924590, 56.29948385550240886, 6.458785618021043895 ) ) ;
#4079 = LINE ( 'NONE', #4933, #10199 ) ;
#4080 = B_SPLINE_CURVE_WITH_KNOTS ( 'NONE', 3,
 ( #8086, #10908, #1425, #3591 ),
 .UNSPECIFIED., .F., .F.,
 ( 4, 4 ),
 ( 2.380739282773774244E-07, 0.002044882221487524104 ),
 .UNSPECIFIED. ) ;
#4081 = CARTESIAN_POINT ( 'NONE',  ( 14.14213562373094923, -14.99999999999999112, -23.00000000000000000 ) ) ;
#4082 = AXIS2_PLACEMENT_3D ( 'NONE', #8331, #5084, #2998 ) ;
#4083 = CARTESIAN_POINT ( 'NONE',  ( 45.27934281921075410, 51.29948385550240175, -6.458785618021043895 ) ) ;
#4084 = EDGE_LOOP ( 'NONE', ( #8343, #1715, #8828 ) ) ;
#4085 = AXIS2_PLACEMENT_3D ( 'NONE', #9037, #5802, #9998 ) ;
#4086 = EDGE_LOOP ( 'NONE', ( #9172, #12991, #12937, #1607 ) ) ;
#4087 = ORIENTED_EDGE ( 'NONE', *, *, #5599, .F. ) ;
#4088 = DIRECTION ( 'NONE',  ( 0.000000000000000000, 0.000000000000000000, 1.000000000000000000 ) ) ;
#4089 = ADVANCED_FACE ( 'NONE', ( #3904 ), #5027, .T. ) ;
#4090 = EDGE_CURVE ( 'NONE', #7440, #9688, #10196, .T. ) ;
#4091 = AXIS2_PLACEMENT_3D ( 'NONE', #8441, #7413, #11619 ) ;
#4092 = DIRECTION ( 'NONE',  ( 0.000000000000000000, -0.000000000000000000, 1.000000000000000000 ) ) ;
#4093 = CARTESIAN_POINT ( 'NONE',  ( 6.242800618755128816, -3.923709308886856206, 3.414402460854895072 ) ) ;
#4094 = CARTESIAN_POINT ( 'NONE',  ( 13.99999999999999822, 1.971681346627238735E-16, -1.610000000000000098 ) ) ;
#4095 = CARTESIAN_POINT ( 'NONE',  ( 48.07319477248762496, 46.40051614449765793, -6.007379884777208190 ) ) ;
#4096 = EDGE_CURVE ( 'NONE', #6800, #12479, #3408, .T. ) ;
#4097 = CARTESIAN_POINT ( 'NONE',  ( 50.02271294988505446, 60.50051614449765935, -7.000000000000000888 ) ) ;
#4098 = CARTESIAN_POINT ( 'NONE',  ( 41.58830220609386430, 60.00051614449765935, -0.02388180880514929535 ) ) ;
#4099 = CARTESIAN_POINT ( 'NONE',  ( 3.999999999999999112, 1.941961291383486277, -0.3515519931180248192 ) ) ;
#4100 = CARTESIAN_POINT ( 'NONE',  ( 52.62207051974829852, 50.60051614449765367, -7.992620115222797139 ) ) ;
#4102 = ORIENTED_EDGE ( 'NONE', *, *, #12746, .F. ) ;
#4101 = ORIENTED_EDGE ( 'NONE', *, *, #11505, .T. ) ;
#4103 = ORIENTED_EDGE ( 'NONE', *, *, #10500, .F. ) ;
#4104 = VERTEX_POINT ( 'NONE', #704 ) ;
#4105 = CARTESIAN_POINT ( 'NONE',  ( 4.071447262713888016, 4.041451884327382338, 0.000000000000000000 ) ) ;
#4106 = PLANE ( 'NONE',  #2157 ) ;
#4107 = CARTESIAN_POINT ( 'NONE',  ( 0.3106000600989267113, 3.122278952918445150, -4.592054218142293642 ) ) ;
#4108 = CARTESIAN_POINT ( 'NONE',  ( 2.449293598294706513E-15, -20.00000000000000000, 9.000000000000000000 ) ) ;
#4109 = PRODUCT_CONTEXT ( 'NONE', #4778, 'mechanical' ) ;
#4110 = CARTESIAN_POINT ( 'NONE',  ( 49.97728705011488159, 65.49948385550240459, -7.000000000000000888 ) ) ;
#4111 = CARTESIAN_POINT ( 'NONE',  ( 45.86712807150323812, 61.29948385550240886, -5.649768623646098220 ) ) ;
#4112 = CARTESIAN_POINT ( 'NONE',  ( 42.63976443033212860, 60.00051614449764514, -0.02388180880514948964 ) ) ;
#4113 = CARTESIAN_POINT ( 'NONE',  ( 0.000000000000000000, 0.000000000000000000, 3.469446951953614189E-15 ) ) ;
#4114 = LINE ( 'NONE', #4043, #782 ) ;
#4115 = EDGE_CURVE ( 'NONE', #1787, #11356, #5856, .T. ) ;
#4116 = CARTESIAN_POINT ( 'NONE',  ( 42.63976443033212860, 52.00051614449766646, -0.02388180880514948964 ) ) ;
#4117 = CARTESIAN_POINT ( 'NONE',  ( 55.11794222512601493, 52.19948385550240744, 3.688883143319541702 ) ) ;
#4118 = CARTESIAN_POINT ( 'NONE',  ( 4.000000000000000000, -2.309401076758514915, -3.433295621305383349 ) ) ;
#4119 = EDGE_LOOP ( 'NONE', ( #2349, #3077, #4694, #5133 ) ) ;
#4120 = CARTESIAN_POINT ( 'NONE',  ( 5.599999999999999645, 4.041451884327382338, 0.000000000000000000 ) ) ;
#4121 = ORIENTED_EDGE ( 'NONE', *, *, #4329, .F. ) ;
#4122 = ORIENTED_EDGE ( 'NONE', *, *, #2013, .T. ) ;
#4123 = CARTESIAN_POINT ( 'NONE',  ( 4.151274195509678577, -2.039912954708747339, -3.533232880573492274 ) ) ;
#4124 = AXIS2_PLACEMENT_3D ( 'NONE', #4738, #5917, #6810 ) ;
#4125 = PRODUCT_DEFINITION_SHAPE ( 'NONE', 'NONE',  #10465 ) ;
#4126 = DIRECTION ( 'NONE',  ( 1.000000000000000000, 0.000000000000000000, 0.000000000000000000 ) ) ;
#4127 = ADVANCED_FACE ( 'NONE', ( #4955 ), #3698, .F. ) ;
#4128 = DIRECTION ( 'NONE',  ( 4.082155997157843695E-16, -1.000000000000000000, 0.000000000000000000 ) ) ;
#4129 =( LENGTH_UNIT ( ) NAMED_UNIT ( * ) SI_UNIT ( .MILLI., .METRE. ) );
#4130 = DIRECTION ( 'NONE',  ( 0.03086419753086420623, -0.9995235871707959241, 0.000000000000000000 ) ) ;
#4131 = CARTESIAN_POINT ( 'NONE',  ( 53.50833635130544508, 53.30051614449767072, 4.867452303228181343 ) ) ;
#4132 = CARTESIAN_POINT ( 'NONE',  ( 6.196878017913830305, -3.367876570272811509, 4.166666666666666963 ) ) ;
#4133 = CARTESIAN_POINT ( 'NONE',  ( 3.999999999999999112, -0.3979232138631231819, -5.929230630780099908E-17 ) ) ;
#4134 = CARTESIAN_POINT ( 'NONE',  ( 44.05948171654949874, 54.79948385550241596, 4.345558710429105354 ) ) ;
#4135 = EDGE_LOOP ( 'NONE', ( #11354, #12004, #6285, #5584, #12786, #6442 ) ) ;
#4136 = CARTESIAN_POINT ( 'NONE',  ( 44.05948171654949874, 52.79948385550240175, 4.345558710429105354 ) ) ;
#4137 = PRODUCT_RELATED_PRODUCT_CATEGORY ( 'part', '', ( #4005 ) ) ;
#4138 = ORIENTED_EDGE ( 'NONE', *, *, #3391, .F. ) ;
#4139 = CARTESIAN_POINT ( 'NONE',  ( 4.158921784487744411, 2.089935040870091409, 3.500000000000000444 ) ) ;
#4140 = CARTESIAN_POINT ( 'NONE',  ( -11.49038105676654453, -27.50000000000006040, -9.000000000000000000 ) ) ;
#4141 = CARTESIAN_POINT ( 'NONE',  ( 3.973514160553462737, -3.435084588004193140, 1.181876024140318782 ) ) ;
#4142 = DIRECTION ( 'NONE',  ( 0.000000000000000000, 1.000000000000000000, 0.000000000000000000 ) ) ;
#4143 = CARTESIAN_POINT ( 'NONE',  ( 46.49166364869456913, 64.30051614449766362, -4.867452303228181343 ) ) ;
#4144 = CARTESIAN_POINT ( 'NONE',  ( 6.534838248920900483, -5.903531555104836848, 4.671345613696493211E-16 ) ) ;
#4145 = CARTESIAN_POINT ( 'NONE',  ( 42.39856655714566358, 64.89948385550239607, 2.493737253992119207 ) ) ;
#4146 = PRESENTATION_STYLE_ASSIGNMENT (( #7002 ) ) ;
#4147 = CARTESIAN_POINT ( 'NONE',  ( 57.61547081786812896, 58.09948385550241312, 2.450534656007040901 ) ) ;
#4148 = ADVANCED_FACE ( 'NONE', ( #12201 ), #2657, .T. ) ;
#4149 = VERTEX_POINT ( 'NONE', #8063 ) ;
#4150 = ORIENTED_EDGE ( 'NONE', *, *, #12102, .T. ) ;
#4151 = DIRECTION ( 'NONE',  ( 0.5000000000000103251, -0.8660254037844327124, 0.000000000000000000 ) ) ;
#4152 = VECTOR ( 'NONE', #2471, 1000.000000000000114 ) ;
#4153 = CARTESIAN_POINT ( 'NONE',  ( 7.900000000000002132, 9.674709713264094059E-16, -7.900000000000002132 ) ) ;
#4154 = CARTESIAN_POINT ( 'NONE',  ( 6.362374563307726660, -5.433808049138435514, 0.8060918076010795685 ) ) ;
#4155 = CARTESIAN_POINT ( 'NONE',  ( 6.244297270354684848, -1.798312406574552930E-11, -5.105276777067894400 ) ) ;
#4156 = CARTESIAN_POINT ( 'NONE',  ( 53.54508667620424234, 46.70051614449766220, -4.840751629271188961 ) ) ;
#4157 = CARTESIAN_POINT ( 'NONE',  ( 57.36023556966787851, 63.00051614449767357, 0.02388180880515038476 ) ) ;
#4158 = EDGE_CURVE ( 'NONE', #1302, #1843, #10119, .T. ) ;
#4159 = CARTESIAN_POINT ( 'NONE',  ( 45.27934281921075410, 47.29948385550241596, -6.458785618021043895 ) ) ;
#4160 = CARTESIAN_POINT ( 'NONE',  ( 1.250000000000000000, -6.429618962271402616, -1.000000000000000000 ) ) ;
#4161 = EDGE_CURVE ( 'NONE', #10246, #7551, #7607, .T. ) ;
#4162 = CARTESIAN_POINT ( 'NONE',  ( 47.37792948025170858, 49.60051614449766788, 7.992620115222797139 ) ) ;
#4163 = EDGE_CURVE ( 'NONE', #11255, #5890, #13090, .T. ) ;
#4164 = CIRCLE ( 'NONE', #8582, 2.000000000000000888 ) ;
#4165 = ORIENTED_EDGE ( 'NONE', *, *, #6018, .F. ) ;
#4166 = ORIENTED_EDGE ( 'NONE', *, *, #4226, .T. ) ;
#4167 = ORIENTED_EDGE ( 'NONE', *, *, #5970, .F. ) ;
#4168 = CARTESIAN_POINT ( 'NONE',  ( 6.481779955677436256, 5.820445026626583918, -1.884471986315529758E-16 ) ) ;
#4169 = ADVANCED_FACE ( 'NONE', ( #7092, #1540 ), #12134, .T. ) ;
#4170 = CARTESIAN_POINT ( 'NONE',  ( 2.000000000000000000, 1.773042676681340524, -2.059984127722458425E-15 ) ) ;
#4171 = LINE ( 'NONE', #8394, #10471 ) ;
#4172 = DIRECTION ( 'NONE',  ( -0.000000000000000000, 0.000000000000000000, -1.000000000000000000 ) ) ;
#4173 = CARTESIAN_POINT ( 'NONE',  ( 55.71335778527780747, 48.09948385550240602, 1.832500667257165983 ) ) ;
#4174 = CIRCLE ( 'NONE', #843, 1.500000000000000666 ) ;
#4175 = CARTESIAN_POINT ( 'NONE',  ( 56.65037692655918988, 63.89948385550239607, -2.184720259617163762 ) ) ;
#4176 = CARTESIAN_POINT ( 'NONE',  ( 44.05948171654945611, 62.20051614449764799, -4.345558710429044069 ) ) ;
#4177 = AXIS2_PLACEMENT_3D ( 'NONE', #11742, #2396, #12643 ) ;
#4178 = LINE ( 'NONE', #8402, #9973 ) ;
#4179 = CYLINDRICAL_SURFACE ( 'NONE', #13597, 1.500000000000001332 ) ;
#4180 = EDGE_CURVE ( 'NONE', #1211, #8256, #4074, .T. ) ;
#4181 = CARTESIAN_POINT ( 'NONE',  ( 3.961551342853669944, 3.742715940867779700, -0.5174258321190529086 ) ) ;
#4182 = CARTESIAN_POINT ( 'NONE',  ( 55.96859303347802239, 50.80051614449766362, -4.306917132069484566 ) ) ;
#4183 = CARTESIAN_POINT ( 'NONE',  ( 50.02271294988511841, 58.49948385550241170, 6.000000000000000888 ) ) ;
#4184 = DIRECTION ( 'NONE',  ( -0.000000000000000000, -0.000000000000000000, -1.000000000000000000 ) ) ;
#4185 = EDGE_CURVE ( 'NONE', #7204, #9705, #5403, .T. ) ;
#4186 = VERTEX_POINT ( 'NONE', #3075 ) ;
#4187 = COLOUR_RGB ( '',1.000000000000000000, 0.9490196078431372140, 0.9098039215686274384 ) ;
#4188 = CARTESIAN_POINT ( 'NONE',  ( 2.449293598294706513E-15, -20.00000000000000000, -8.999999999999998224 ) ) ;
#4189 = VERTEX_POINT ( 'NONE', #7310 ) ;
#4190 = CARTESIAN_POINT ( 'NONE',  ( 6.534533895392294234, 2.951347675328725106, 5.111884124469659341 ) ) ;
#4191 = CARTESIAN_POINT ( 'NONE',  ( 3.020236159542449172, -23.98474259401938014, -9.999999999999994671 ) ) ;
#4192 = CARTESIAN_POINT ( 'NONE',  ( 4.175813232069146785, 2.061359961916365613, -3.570380186727397653 ) ) ;
#4193 = CARTESIAN_POINT ( 'NONE',  ( 42.63976443033212860, 52.99948385550240459, 0.02388180880522514787 ) ) ;
#4194 = PRODUCT_DEFINITION_FORMATION_WITH_SPECIFIED_SOURCE ( 'ANY', '', #13599, .NOT_KNOWN. ) ;
#4195 = CIRCLE ( 'NONE', #10398, 5.000000000000000000 ) ;
#4196 = CARTESIAN_POINT ( 'NONE',  ( -0.5276280594146446346, 4.314175951381965746, -3.320322319201721495 ) ) ;
#4197 = CARTESIAN_POINT ( 'NONE',  ( 55.08986747509849380, 53.20051614449766220, 3.727524721679155384 ) ) ;
#4198 = CARTESIAN_POINT ( 'NONE',  ( -62.49999999999997158, 32.50000000000001421, 9.999999999999998224 ) ) ;
#4199 = CARTESIAN_POINT ( 'NONE',  ( -74.99999999999997158, -7.499999999999971578, -20.00000000000000000 ) ) ;
#4200 = CARTESIAN_POINT ( 'NONE',  ( 52.29715082351547295, 60.39948385550239607, 6.992620115222774047 ) ) ;
#4201 = CARTESIAN_POINT ( 'NONE',  ( 47.70284917648453415, 57.39948385550241028, -6.992620115222774047 ) ) ;
#4202 = EDGE_CURVE ( 'NONE', #6833, #11747, #9373, .T. ) ;
#4203 = ORIENTED_EDGE ( 'NONE', *, *, #4158, .T. ) ;
#4204 = ORIENTED_EDGE ( 'NONE', *, *, #7972, .T. ) ;
#4205 = CARTESIAN_POINT ( 'NONE',  ( 4.175326769692857987, 4.121399112977855772, 3.964526709274768569E-16 ) ) ;
#4206 = VECTOR ( 'NONE', #12147, 1000.000000000000000 ) ;
#4207 = FACE_OUTER_BOUND ( 'NONE', #9744, .T. ) ;
#4208 = PLANE ( 'NONE',  #4663 ) ;
#4209 = CARTESIAN_POINT ( 'NONE',  ( 62.49999999999998579, 5.000000000000018652, -5.000000000000000000 ) ) ;
#4210 = CARTESIAN_POINT ( 'NONE',  ( 43.34962307344081012, 48.89948385550240317, 2.184720259617164650 ) ) ;
#4211 = CARTESIAN_POINT ( 'NONE',  ( 56.66441430157294690, 44.90051614449765793, -2.141517661632166281 ) ) ;
#4212 = FACE_OUTER_BOUND ( 'NONE', #3552, .T. ) ;
#4213 = CARTESIAN_POINT ( 'NONE',  ( 52.25172492374522903, 45.59948385550240602, -7.007379884777225953 ) ) ;
#4214 = VECTOR ( 'NONE', #3611, 1000.000000000000000 ) ;
#4215 = AXIS2_PLACEMENT_3D ( 'NONE', #5674, #2476, #2545 ) ;
#4216 = CARTESIAN_POINT ( 'NONE',  ( 41.58830220609386430, 54.99948385550239749, 0.02388180880523263147 ) ) ;
#4217 = ORIENTED_EDGE ( 'NONE', *, *, #6291, .T. ) ;
#4218 = VERTEX_POINT ( 'NONE', #6139 ) ;
#4219 = EDGE_CURVE ( 'NONE', #4643, #12840, #4296, .T. ) ;
#4220 = CARTESIAN_POINT ( 'NONE',  ( 12.50000000000000000, 15.00000000000001776, -9.000000000000000000 ) ) ;
#4221 = CARTESIAN_POINT ( 'NONE',  ( -74.99999999999997158, -39.99999999999998579, -20.00000000000000000 ) ) ;
#4222 = DIRECTION ( 'NONE',  ( 1.000000000000000000, 0.000000000000000000, 0.000000000000000000 ) ) ;
#4223 = CARTESIAN_POINT ( 'NONE',  ( 0.000000000000000000, 0.000000000000000000, -4.974599999999998801 ) ) ;
#4224 = CARTESIAN_POINT ( 'NONE',  ( 46.49166364869456913, 48.30051614449765651, -4.867452303228181343 ) ) ;
#4225 = CARTESIAN_POINT ( 'NONE',  ( 43.34962307344078880, 60.10051614449766078, -2.184720259617096705 ) ) ;
#4226 = EDGE_CURVE ( 'NONE', #9486, #3385, #1858, .T. ) ;
#4227 = CARTESIAN_POINT ( 'NONE',  ( 43.20883090819745576, 48.79948385550240175, 4.963592699179006473 ) ) ;
#4228 = CARTESIAN_POINT ( 'NONE',  ( 4.180231891692618440, 2.049421325483208101, 3.591231015387272851 ) ) ;
#4229 = CARTESIAN_POINT ( 'NONE',  ( 43.18075615816994173, 57.80051614449766362, 4.924951120819380357 ) ) ;
#4230 = AXIS2_PLACEMENT_3D ( 'NONE', #447, #12691, #10760 ) ;
#4231 = ORIENTED_EDGE ( 'NONE', *, *, #2139, .F. ) ;
#4232 = VERTEX_POINT ( 'NONE', #8271 ) ;
#4233 = ORIENTED_EDGE ( 'NONE', *, *, #585, .T. ) ;
#4234 = DIRECTION ( 'NONE',  ( 0.000000000000000000, 0.000000000000000000, -1.000000000000000000 ) ) ;
#4235 = DIRECTION ( 'NONE',  ( -0.000000000000000000, 0.000000000000000000, -1.000000000000000000 ) ) ;
#4236 = ADVANCED_FACE ( 'NONE', ( #1047 ), #2034, .T. ) ;
#4237 = DIRECTION ( 'NONE',  ( 0.000000000000000000, 0.000000000000000000, 1.000000000000000000 ) ) ;
#4238 = CARTESIAN_POINT ( 'NONE',  ( -4.000000000000000888, -2.309401076758512694, -3.504269196027526512 ) ) ;
#4239 = AXIS2_PLACEMENT_3D ( 'NONE', #11916, #12942, #3486 ) ;
#4240 = EDGE_CURVE ( 'NONE', #8931, #13447, #11644, .T. ) ;
#4241 = CARTESIAN_POINT ( 'NONE',  ( 43.69122665457040000, 52.99948385550241170, 0.02388180880521036456 ) ) ;
#4242 = AXIS2_PLACEMENT_3D ( 'NONE', #12250, #9406, #10033 ) ;
#4243 = CARTESIAN_POINT ( 'NONE',  ( 54.09612160359786515, 63.69948385550240744, -5.676469297603166098 ) ) ;
#4244 = CIRCLE ( 'NONE', #7993, 12.49999999999999645 ) ;
#4245 = CARTESIAN_POINT ( 'NONE',  ( 42.39856655714564226, 46.10051614449766078, -2.493737253992044156 ) ) ;
#4246 = LINE ( 'NONE', #8464, #5347 ) ;
#4247 = CARTESIAN_POINT ( 'NONE',  ( 0.000000000000000000, -1.773042676681341856, 2.276824562219559311E-15 ) ) ;
#4248 = CARTESIAN_POINT ( 'NONE',  ( 3.309651814758565180, -5.455921364805393026, 0.000000000000000000 ) ) ;
#4249 = CARTESIAN_POINT ( 'NONE',  ( 45.86712807150329496, 57.70051614449765509, 5.649768623646139964 ) ) ;
#4250 = CARTESIAN_POINT ( 'NONE',  ( 48.02776887271745210, 57.39948385550241028, -5.992620115222778487 ) ) ;
#4251 = B_SPLINE_CURVE_WITH_KNOTS ( 'NONE', 3,
 ( #2507, #12239, #1387, #3876 ),
 .UNSPECIFIED., .F., .F.,
 ( 4, 4 ),
 ( 2.380735203086575858E-07, 0.002921158011986710323 ),
 .UNSPECIFIED. ) ;
#4252 = CARTESIAN_POINT ( 'NONE',  ( 0.000000000000000000, 0.000000000000000000, 0.000000000000000000 ) ) ;
#4253 = ORIENTED_EDGE ( 'NONE', *, *, #4923, .F. ) ;
#4254 = VECTOR ( 'NONE', #9105, 1000.000000000000000 ) ;
#4255 = DIRECTION ( 'NONE',  ( -0.000000000000000000, -0.000000000000000000, -1.000000000000000000 ) ) ;
#4256 = ORIENTED_EDGE ( 'NONE', *, *, #9890, .T. ) ;
#4257 = CARTESIAN_POINT ( 'NONE',  ( 6.452281807715809059, 2.898928808472990060, 5.021091983800332947 ) ) ;
#4258 =( REPRESENTATION_RELATIONSHIP ('NONE','NONE', #5328, #3897 ) REPRESENTATION_RELATIONSHIP_WITH_TRANSFORMATION ( #10188 )SHAPE_REPRESENTATION_RELATIONSHIP( ) );
#4259 = VECTOR ( 'NONE', #4774, 999.9999999999998863 ) ;
#4260 = CARTESIAN_POINT ( 'NONE',  ( 2.899426713160750069, -23.82535289025860337, -8.999999999999996447 ) ) ;
#4261 = CARTESIAN_POINT ( 'NONE',  ( -62.49999999999997158, 32.50000000000001421, 15.00000000000000000 ) ) ;
#4262 = EDGE_CURVE ( 'NONE', #9574, #651, #739, .T. ) ;
#4263 = DIRECTION ( 'NONE',  ( 1.000000000000000000, 0.000000000000000000, 0.000000000000000000 ) ) ;
#4264 = CARTESIAN_POINT ( 'NONE',  ( 45.86712807150323812, 51.29948385550240175, -5.649768623646098220 ) ) ;
#4265 = EDGE_CURVE ( 'NONE', #8586, #7290, #10909, .T. ) ;
#4266 = CARTESIAN_POINT ( 'NONE',  ( -2.712762565639006418, 3.052587955997511759, -3.430618716626627318 ) ) ;
#4267 = CARTESIAN_POINT ( 'NONE',  ( 55.11794222512599362, 54.80051614449764941, -3.688883143319583446 ) ) ;
#4268 = CARTESIAN_POINT ( 'NONE',  ( -4.000000000000000000, 0.000000000000000000, 0.000000000000000000 ) ) ;
#4269 = DIRECTION ( 'NONE',  ( 1.000000000000000000, -0.000000000000000000, 0.000000000000000000 ) ) ;
#4270 = CARTESIAN_POINT ( 'NONE',  ( 0.02993401039713615083, 3.373851915354614928, 1.156317065392238774 ) ) ;
#4271 = CARTESIAN_POINT ( 'NONE',  ( 44.05948171654949874, 58.79948385550240886, 4.345558710429105354 ) ) ;
#4272 = AXIS2_PLACEMENT_3D ( 'NONE', #10918, #2764, #10848 ) ;
#4273 = EDGE_LOOP ( 'NONE', ( #8712, #9484, #11522, #5387 ) ) ;
#4274 = VERTEX_POINT ( 'NONE', #3216 ) ;
#4275 = CARTESIAN_POINT ( 'NONE',  ( -74.99999999999997158, 20.00000000000001421, 15.00000000000000000 ) ) ;
#4276 = DIRECTION ( 'NONE',  ( 1.000000000000000000, 0.000000000000000000, 0.000000000000000000 ) ) ;
#4277 = DIRECTION ( 'NONE',  ( 0.000000000000000000, 0.000000000000000000, -1.000000000000000000 ) ) ;
#4278 = FACE_BOUND ( 'NONE', #9027, .T. ) ;
#4279 = CARTESIAN_POINT ( 'NONE',  ( 42.63976443033212149, 48.99948385550241170, 0.02388180880522514787 ) ) ;
#4280 = CARTESIAN_POINT ( 'NONE',  ( 50.02271294988505446, 50.50051614449765935, -7.000000000000000888 ) ) ;
#4281 = DIRECTION ( 'NONE',  ( -1.000000000000000000, 9.251858538542972814E-17, -0.000000000000000000 ) ) ;
#4282 = CARTESIAN_POINT ( 'NONE',  ( 41.58830220609386430, 62.99948385550241170, 0.02388180880523263147 ) ) ;
#4283 = DIRECTION ( 'NONE',  ( 0.000000000000000000, 0.000000000000000000, 1.000000000000000000 ) ) ;
#4284 = CARTESIAN_POINT ( 'NONE',  ( 57.61547081786812896, 56.09948385550240602, 2.450534656007040901 ) ) ;
#4285 = AXIS2_PLACEMENT_3D ( 'NONE', #3352, #2305, #1251 ) ;
#4286 = ORIENTED_EDGE ( 'NONE', *, *, #4219, .T. ) ;
#4287 = ORIENTED_EDGE ( 'NONE', *, *, #11603, .F. ) ;
#4288 = CARTESIAN_POINT ( 'NONE',  ( -1.000000000000000000, -14.00000000000000000, 8.999999999999998224 ) ) ;
#4289 = B_SPLINE_CURVE_WITH_KNOTS ( 'NONE', 3,
 ( #13595, #1848, #10289, #4141, #11397, #5260 ),
 .UNSPECIFIED., .F., .F.,
 ( 4, 2, 4 ),
 ( 0.000000000000000000, 0.002086519881787261485, 0.004173039763574522970 ),
 .UNSPECIFIED. ) ;
#4290 = CARTESIAN_POINT ( 'NONE',  ( 6.245824673232967861, -4.939548505213401164, 1.655093584844986143 ) ) ;
#4291 = CARTESIAN_POINT ( 'NONE',  ( 2.836893136758676270, 3.208949435745843903, -3.505054077164911241 ) ) ;
#4292 = CARTESIAN_POINT ( 'NONE',  ( 55.71335778527780036, 48.90051614449766504, -1.832500667257213056 ) ) ;
#4293 = CARTESIAN_POINT ( 'NONE',  ( 44.03140696652198471, 59.80051614449766362, 4.306917132069485454 ) ) ;
#4294 = CARTESIAN_POINT ( 'NONE',  ( 56.79116909180255135, 45.79948385550240886, -4.963592699179005585 ) ) ;
#4295 = CARTESIAN_POINT ( 'NONE',  ( 50.00000000000000000, 15.00000000000000000, 0.000000000000000000 ) ) ;
#4296 = CIRCLE ( 'NONE', #12677, 4.800000000000000711 ) ;
#4297 = CARTESIAN_POINT ( 'NONE',  ( 57.60143344285435774, 55.10051614449765367, 2.493737253992045044 ) ) ;
#4298 = ADVANCED_FACE ( 'NONE', ( #13635 ), #13550, .F. ) ;
#4299 = CIRCLE ( 'NONE', #3854, 4.999999999999999112 ) ;
#4300 = VERTEX_POINT ( 'NONE', #9505 ) ;
#4301 = EDGE_LOOP ( 'NONE', ( #10520, #13620, #3858, #1629 ) ) ;
#4302 = EDGE_LOOP ( 'NONE', ( #2837, #12907, #1371, #5774, #13187 ) ) ;
#4303 = PRODUCT_RELATED_PRODUCT_CATEGORY ( 'part', '', ( #3464 ) ) ;
#4304 = CIRCLE ( 'NONE', #11809, 5.000000000000000000 ) ;
#4305 = CARTESIAN_POINT ( 'NONE',  ( 6.506987859255521478, 5.850751062354592413, 1.196609732200561596E-15 ) ) ;
#4306 = FACE_OUTER_BOUND ( 'NONE', #7074, .T. ) ;
#4307 = FACE_OUTER_BOUND ( 'NONE', #10089, .T. ) ;
#4308 = CARTESIAN_POINT ( 'NONE',  ( -62.49999999999997158, 45.00000000000001421, 15.00000000000000000 ) ) ;
#4309 = LINE ( 'NONE', #12046, #5826 ) ;
#4310 = CARTESIAN_POINT ( 'NONE',  ( 46.45491332379572924, 47.29948385550241596, -4.840751629271157874 ) ) ;
#4311 = CARTESIAN_POINT ( 'NONE',  ( 55.94051828345050836, 63.79948385550240886, -4.345558710429103577 ) ) ;
#4312 = CARTESIAN_POINT ( 'NONE',  ( 54.68390685589039890, 47.30051614449766362, 6.485486291978072693 ) ) ;
#4313 = CARTESIAN_POINT ( 'NONE',  ( 1.925929944387235853E-31, 15.00000000000001599, 9.000000000000000000 ) ) ;
#4314 = CARTESIAN_POINT ( 'NONE',  ( 2.000000000000000000, 1.773042676681340524, -2.059984127722458425E-15 ) ) ;
#4315 = CIRCLE ( 'NONE', #4956, 1.499999999999999334 ) ;
#4316 = CARTESIAN_POINT ( 'NONE',  ( 43.33558569842706021, 57.90051614449766504, 2.141517661632167169 ) ) ;
#4317 = CARTESIAN_POINT ( 'NONE',  ( 55.69932041026404335, 57.89948385550241028, -1.875703265242203432 ) ) ;
#4318 = FACE_OUTER_BOUND ( 'NONE', #2263, .T. ) ;
#4319 = ORIENTED_EDGE ( 'NONE', *, *, #5252, .T. ) ;
#4320 = CARTESIAN_POINT ( 'NONE',  ( 0.1481481481481481122, -4.797713218419819903, -1.000000000000000000 ) ) ;
#4321 = ORIENTED_EDGE ( 'NONE', *, *, #3067, .T. ) ;
#4322 = CARTESIAN_POINT ( 'NONE',  ( 0.000000000000000000, 1.773042676681340524, -2.059984127722458425E-15 ) ) ;
#4323 = DIRECTION ( 'NONE',  ( 1.000000000000000000, 0.000000000000000000, 0.000000000000000000 ) ) ;
#4324 = EDGE_CURVE ( 'NONE', #8026, #3586, #12888, .T. ) ;
#4325 = LINE ( 'NONE', #10615, #11944 ) ;
#4326 = CARTESIAN_POINT ( 'NONE',  ( 52.29715082351547295, 52.39948385550241738, 6.992620115222774047 ) ) ;
#4327 = CARTESIAN_POINT ( 'NONE',  ( 2.649999999999988365, 15.00000000000001599, -9.999999999999998224 ) ) ;
#4328 = CARTESIAN_POINT ( 'NONE',  ( 44.28664221472221385, 51.90051614449765793, 1.832500667257213722 ) ) ;
#4329 = EDGE_CURVE ( 'NONE', #1843, #11056, #310, .T. ) ;
#4330 = CARTESIAN_POINT ( 'NONE',  ( 4.175326769692855322, -2.060699556488924333, 3.569236330973470928 ) ) ;
#4331 = CARTESIAN_POINT ( 'NONE',  ( 44.05948171654949874, 62.79948385550241596, 4.345558710429105354 ) ) ;
#4332 = CARTESIAN_POINT ( 'NONE',  ( -62.49999999999997158, 32.50000000000001421, 10.00000000000000000 ) ) ;
#4333 = CARTESIAN_POINT ( 'NONE',  ( 43.33558569842703179, 59.09948385550240602, -2.141517661632099223 ) ) ;
#4334 = FACE_OUTER_BOUND ( 'NONE', #7688, .T. ) ;
#4335 = ORIENTED_EDGE ( 'NONE', *, *, #11163, .F. ) ;
#4336 = EDGE_CURVE ( 'NONE', #13537, #4887, #6209, .T. ) ;
#4337 = CIRCLE ( 'NONE', #8322, 0.5155456020628804703 ) ;
#4338 = ADVANCED_FACE ( 'NONE', ( #28 ), #7375, .T. ) ;
#4339 = VECTOR ( 'NONE', #2164, 1000.000000000000000 ) ;
#4340 = ORIENTED_EDGE ( 'NONE', *, *, #8568, .F. ) ;
#4341 = ORIENTED_EDGE ( 'NONE', *, *, #5151, .T. ) ;
#4342 = CARTESIAN_POINT ( 'NONE',  ( 4.071447262713888016, 4.041451884327382338, 0.000000000000000000 ) ) ;
#4343 = DIRECTION ( 'NONE',  ( 0.000000000000000000, 0.000000000000000000, -1.000000000000000000 ) ) ;
#4344 = DIRECTION ( 'NONE',  ( -0.000000000000000000, -0.000000000000000000, -1.000000000000000000 ) ) ;
#4345 = DIRECTION ( 'NONE',  ( 1.000000000000000000, 0.000000000000000000, -0.000000000000000000 ) ) ;
#4346 = CARTESIAN_POINT ( 'NONE',  ( 50.02271294988512551, 50.49948385550240459, 7.000000000000000888 ) ) ;
#4347 = CARTESIAN_POINT ( 'NONE',  ( 54.13287192849671214, 48.70051614449766220, -5.649768623646139964 ) ) ;
#4348 = DIRECTION ( 'NONE',  ( 1.000000000000000000, 0.000000000000000000, 0.000000000000000000 ) ) ;
#4349 = CARTESIAN_POINT ( 'NONE',  ( 45.27934281921075410, 65.29948385550241596, -6.458785618021043895 ) ) ;
#4350 = AXIS2_PLACEMENT_3D ( 'NONE', #6793, #9765, #1515 ) ;
#4351 = DIRECTION ( 'NONE',  ( -1.000000000000000000, 0.000000000000000000, 0.000000000000000000 ) ) ;
#4352 = CARTESIAN_POINT ( 'NONE',  ( 43.20883090819745576, 54.79948385550240175, 4.963592699179006473 ) ) ;
#4353 = ORIENTED_EDGE ( 'NONE', *, *, #12603, .T. ) ;
#4354 = ORIENTED_EDGE ( 'NONE', *, *, #12989, .F. ) ;
#4355 = CARTESIAN_POINT ( 'NONE',  ( 2.649999999999988365, 15.00000000000001599, 15.00000000000000000 ) ) ;
#4356 = EDGE_CURVE ( 'NONE', #8026, #8586, #8049, .T. ) ;
#4357 = CARTESIAN_POINT ( 'NONE',  ( 0.3126073911696451990, -4.041451884327386779, -1.834154111220703958E-17 ) ) ;
#4358 = CARTESIAN_POINT ( 'NONE',  ( 50.02271294988506156, 48.50051614449765935, -6.000000000000000888 ) ) ;
#4359 = CARTESIAN_POINT ( 'NONE',  ( 55.94051828345054389, 61.20051614449765509, 4.345558710429044957 ) ) ;
#4360 = CARTESIAN_POINT ( 'NONE',  ( 45.31609314410960820, 64.30051614449766362, -6.485486291978072693 ) ) ;
#4361 = CARTESIAN_POINT ( 'NONE',  ( 4.175572532730933872, -4.122058607836120103, 1.048217341165752127E-14 ) ) ;
#4362 = CARTESIAN_POINT ( 'NONE',  ( 56.81924384183006538, 56.80051614449764941, -4.924951120819380357 ) ) ;
#4363 = VERTEX_POINT ( 'NONE', #13573 ) ;
#4364 = ORIENTED_EDGE ( 'NONE', *, *, #6250, .T. ) ;
#4365 = VERTEX_POINT ( 'NONE', #4118 ) ;
#4366 = ORIENTED_EDGE ( 'NONE', *, *, #2896, .T. ) ;
#4367 = DIRECTION ( 'NONE',  ( -0.000000000000000000, -0.000000000000000000, 1.000000000000000000 ) ) ;
#4368 = LINE ( 'NONE', #3610, #3931 ) ;
#4369 = DIRECTION ( 'NONE',  ( -0.000000000000000000, -0.000000000000000000, 1.000000000000000000 ) ) ;
#4370 = CARTESIAN_POINT ( 'NONE',  ( -22.00000000000000000, -19.99999999999999289, -12.00000000000000000 ) ) ;
#4371 = CARTESIAN_POINT ( 'NONE',  ( 0.3208286057739604957, -4.433571671609698228, -0.3503314178412692548 ) ) ;
#4372 = CARTESIAN_POINT ( 'NONE',  ( 51.97223112728254790, 48.39948385550240317, 5.992620115222778487 ) ) ;
#4373 = CARTESIAN_POINT ( 'NONE',  ( 45.86712807150323812, 65.29948385550241596, -5.649768623646098220 ) ) ;
#4374 = CARTESIAN_POINT ( 'NONE',  ( 52.57664461997821093, 45.40051614449765793, 8.007379884777206414 ) ) ;
#4375 = VECTOR ( 'NONE', #5966, 1000.000000000000000 ) ;
#4376 = CARTESIAN_POINT ( 'NONE',  ( 75.00000000000001421, -7.499999999999971578, -20.00000000000000000 ) ) ;
#4377 = DIRECTION ( 'NONE',  ( 0.8660254037844379305, 0.5000000000000013323, 0.000000000000000000 ) ) ;
#4378 = CARTESIAN_POINT ( 'NONE',  ( 44.05948171654945611, 54.20051614449764799, -4.345558710429044069 ) ) ;
#4379 = CARTESIAN_POINT ( 'NONE',  ( 55.69932041026404335, 61.89948385550241738, -1.875703265242203432 ) ) ;
#4380 = ORIENTED_EDGE ( 'NONE', *, *, #10500, .T. ) ;
#4381 = CARTESIAN_POINT ( 'NONE',  ( -7.500000000000013323, -7.009618943233427935, 9.000000000000000000 ) ) ;
#4382 = ORIENTED_EDGE ( 'NONE', *, *, #4677, .F. ) ;
#4383 = DIRECTION ( 'NONE',  ( 1.000000000000000000, 3.469446951953615668E-16, -0.000000000000000000 ) ) ;
#4384 = CIRCLE ( 'NONE', #2383, 4.000000000000000000 ) ;
#4385 = FACE_OUTER_BOUND ( 'NONE', #6922, .T. ) ;
#4386 = CARTESIAN_POINT ( 'NONE',  ( 4.132952817037867987, 2.031684012687259511, -3.518979934899751694 ) ) ;
#4387 = CARTESIAN_POINT ( 'NONE',  ( 42.63976443033212860, 48.99948385550240459, 0.02388180880522514787 ) ) ;
#4388 = CARTESIAN_POINT ( 'NONE',  ( 0.3461262719736147297, -4.658553426539303821, -3.671615880910379381 ) ) ;
#4389 = CARTESIAN_POINT ( 'NONE',  ( 48.07319477248762496, 52.40051614449767214, -6.007379884777208190 ) ) ;
#4390 = ADVANCED_FACE ( 'NONE', ( #4318 ), #11709, .F. ) ;
#4391 = CARTESIAN_POINT ( 'NONE',  ( 4.165266963751724560, -2.049631966911991565, 3.550066703508907739 ) ) ;
#4392 = CARTESIAN_POINT ( 'NONE',  ( -4.999999999999998224, -20.00000000000000000, 9.999999999999998224 ) ) ;
#4393 = CARTESIAN_POINT ( 'NONE',  ( 6.534838248920900483, -5.903531555104836848, 4.671345613696493211E-16 ) ) ;
#4394 = CARTESIAN_POINT ( 'NONE',  ( 56.66441430157296821, 60.09948385550240602, 2.141517661632100111 ) ) ;
#4395 = CARTESIAN_POINT ( 'NONE',  ( 0.08165819712377191120, -4.939961795957299451, -1.443735181952766400 ) ) ;
#4396 = CIRCLE ( 'NONE', #6185, 4.000000000000000000 ) ;
#4397 = EDGE_LOOP ( 'NONE', ( #12005, #3534 ) ) ;
#4398 = AXIS2_PLACEMENT_3D ( 'NONE', #2654, #6878, #12400 ) ;
#4399 = VECTOR ( 'NONE', #1319, 1000.000000000000114 ) ;
#4400 = PRODUCT_DEFINITION_CONTEXT ( 'detailed design', #6128, 'design' ) ;
#4401 = ORIENTED_EDGE ( 'NONE', *, *, #5192, .F. ) ;
#4402 = EDGE_LOOP ( 'NONE', ( #12103, #5187, #10037, #11233, #12579, #11690 ) ) ;
#4403 = DIRECTION ( 'NONE',  ( 0.000000000000000000, 1.000000000000000000, 0.000000000000000000 ) ) ;
#4404 = EDGE_CURVE ( 'NONE', #408, #7877, #2229, .T. ) ;
#4405 = CARTESIAN_POINT ( 'NONE',  ( 3.510273485745307731, 2.827716139362654424, -3.610536846335885564 ) ) ;
#4406 = STYLED_ITEM ( 'NONE', ( #3156 ), #7343 ) ;
#4407 = CARTESIAN_POINT ( 'NONE',  ( 75.00000000000001421, 7.500000000000027534, -10.00000000000000000 ) ) ;
#4408 = VECTOR ( 'NONE', #12163, 1000.000000000000000 ) ;
#4409 = CARTESIAN_POINT ( 'NONE',  ( -4.078421086530219064, -3.990950201428956845, -1.000000000000000000 ) ) ;
#4410 = EDGE_CURVE ( 'NONE', #2434, #5304, #5368, .T. ) ;
#4411 = CARTESIAN_POINT ( 'NONE',  ( 54.09612160359786515, 55.69948385550240744, -5.676469297603166098 ) ) ;
#4412 = CARTESIAN_POINT ( 'NONE',  ( 54.09612160359792199, 53.30051614449766362, 5.676469297603124353 ) ) ;
#4413 = EDGE_CURVE ( 'NONE', #7202, #9377, #3278, .T. ) ;
#4414 = CARTESIAN_POINT ( 'NONE',  ( -8.759913291900476295, -7.823632761846195827, 9.000000000000000000 ) ) ;
#4415 = CARTESIAN_POINT ( 'NONE',  ( 52.29715082351547295, 46.39948385550240317, 6.992620115222774047 ) ) ;
#4416 = SURFACE_SIDE_STYLE ('',( #10708 ) ) ;
#4417 = COLOUR_RGB ( '',1.000000000000000000, 0.9490196078431372140, 0.9098039215686274384 ) ;
#4418 = CARTESIAN_POINT ( 'NONE',  ( 47.37792948025162332, 57.39948385550241028, -7.992620115222770494 ) ) ;
#4419 = AXIS2_PLACEMENT_3D ( 'NONE', #8502, #1074, #947 ) ;
#4420 = EDGE_LOOP ( 'NONE', ( #6211, #2575, #8659, #8992 ) ) ;
#4421 = EDGE_LOOP ( 'NONE', ( #2519, #13394, #3590 ) ) ;
#4422 = CARTESIAN_POINT ( 'NONE',  ( 4.071447262713887127, 2.020725942163688504, 3.500000000000000000 ) ) ;
#4423 = CARTESIAN_POINT ( 'NONE',  ( -4.688877333428352223, -21.02685410450703074, 9.000000000000000000 ) ) ;
#4424 = CARTESIAN_POINT ( 'NONE',  ( 55.71335778527780036, 56.90051614449767214, -1.832500667257213056 ) ) ;
#4425 = AXIS2_PLACEMENT_3D ( 'NONE', #13400, #5897, #10094 ) ;
#4426 = DIRECTION ( 'NONE',  ( 0.000000000000000000, 0.000000000000000000, -1.000000000000000000 ) ) ;
#4427 = CARTESIAN_POINT ( 'NONE',  ( 42.38452918213188525, 49.09948385550241312, -2.450534656007040013 ) ) ;
#4428 = DIRECTION ( 'NONE',  ( 0.000000000000000000, 0.000000000000000000, 1.000000000000000000 ) ) ;
#4429 = CARTESIAN_POINT ( 'NONE',  ( 43.20883090819742023, 54.20051614449766220, -4.963592699178938972 ) ) ;
#4430 = B_SPLINE_CURVE_WITH_KNOTS ( 'NONE', 3,
 ( #4616, #8836, #8001, #12211, #1479, #2740, #11170, #13034, #3578, #12011, #4391, #13019, #5381, #4330, #5646, #9588 ),
 .UNSPECIFIED., .F., .F.,
 ( 4, 3, 3, 3, 3, 4 ),
 ( 0.000000000000000000, 3.315506744709513341E-05, 6.608280158699547874E-05, 0.0001026520855291439131, 0.0001376952025664790686, 0.0001398064759190603148 ),
 .UNSPECIFIED. ) ;
#4431 = ORIENTED_EDGE ( 'NONE', *, *, #7807, .F. ) ;
#4432 = ORIENTED_EDGE ( 'NONE', *, *, #13242, .F. ) ;
#4433 = ORIENTED_EDGE ( 'NONE', *, *, #1650, .T. ) ;
#4434 = ORIENTED_EDGE ( 'NONE', *, *, #12541, .T. ) ;
#4435 = CARTESIAN_POINT ( 'NONE',  ( -3.349226789952655547, -2.685125164760744809, -0.2236248678334863682 ) ) ;
#4436 = DIRECTION ( 'NONE',  ( -1.000000000000000000, 0.000000000000000000, 0.000000000000000000 ) ) ;
#4437 = FACE_BOUND ( 'NONE', #5334, .T. ) ;
#4438 = CARTESIAN_POINT ( 'NONE',  ( 2.649999999999988365, 15.00000000000001599, 9.000000000000000000 ) ) ;
#4439 = EDGE_CURVE ( 'NONE', #4365, #4606, #6007, .T. ) ;
#4440 = CARTESIAN_POINT ( 'NONE',  ( -31.74999999999995737, 0.000000000000000000, 0.000000000000000000 ) ) ;
#4441 = CARTESIAN_POINT ( 'NONE',  ( 56.30877334542961421, 51.99948385550239749, -0.02388180880520959434 ) ) ;
#4442 = CARTESIAN_POINT ( 'NONE',  ( 52.25172492374528588, 47.40051614449765793, 7.007379884777204637 ) ) ;
#4443 = CARTESIAN_POINT ( 'NONE',  ( 56.81924384183006538, 48.80051614449767072, -4.924951120819380357 ) ) ;
#4444 = CARTESIAN_POINT ( 'NONE',  ( 8.500000000000000000, 2.886751345948125991, 4.999999999999999112 ) ) ;
#4445 = CARTESIAN_POINT ( 'NONE',  ( 3.309651814758564736, -5.455921364805393026, -1.000000000000000000 ) ) ;
#4446 = CARTESIAN_POINT ( 'NONE',  ( 49.97728705011495265, 57.50051614449766646, 7.000000000000000888 ) ) ;
#4447 = CARTESIAN_POINT ( 'NONE',  ( 50.02271294988511841, 62.49948385550240459, 6.000000000000000888 ) ) ;
#4448 = ORIENTED_EDGE ( 'NONE', *, *, #1649, .T. ) ;
#4449 = DIRECTION ( 'NONE',  ( 0.000000000000000000, 0.000000000000000000, -1.000000000000000000 ) ) ;
#4450 = EDGE_LOOP ( 'NONE', ( #12237, #8510, #6723, #653 ) ) ;
#4451 = CARTESIAN_POINT ( 'NONE',  ( 6.534838248920897819, 2.951765777552412651, 5.112608298763836601 ) ) ;
#4452 = CIRCLE ( 'NONE', #10198, 9.999999999999998224 ) ;
#4453 = PRODUCT_DEFINITION_SHAPE ( 'NONE', 'NONE',  #13677 ) ;
#4454 = CARTESIAN_POINT ( 'NONE',  ( 4.688877333453707941, -18.97314589549297281, 9.000000000000000000 ) ) ;
#4455 = CIRCLE ( 'NONE', #7548, 4.799999999999999822 ) ;
#4456 = CARTESIAN_POINT ( 'NONE',  ( 4.086262629614029862, -1.979770830881092181, -3.570936333571104626 ) ) ;
#4457 = SURFACE_STYLE_FILL_AREA ( #1057 ) ;
#4458 = CARTESIAN_POINT ( 'NONE',  ( 55.94051828345050836, 49.79948385550240175, -4.345558710429104465 ) ) ;
#4459 = DIRECTION ( 'NONE',  ( 0.000000000000000000, 0.000000000000000000, 1.000000000000000000 ) ) ;
#4460 = CARTESIAN_POINT ( 'NONE',  ( 50.02271294988506156, 56.50051614449767357, -6.000000000000000888 ) ) ;
#4461 = DIRECTION ( 'NONE',  ( -0.000000000000000000, -0.000000000000000000, 1.000000000000000000 ) ) ;
#4462 = LINE ( 'NONE', #10813, #10363 ) ;
#4463 = CARTESIAN_POINT ( 'NONE',  ( 0.1388410611046087539, 3.710337782248032568, 0.5735064479039790886 ) ) ;
#4464 = CARTESIAN_POINT ( 'NONE',  ( 56.66441430157296821, 58.09948385550240602, 2.141517661632100111 ) ) ;
#4465 = AXIS2_PLACEMENT_3D ( 'NONE', #12308, #13542, #1023 ) ;
#4466 = CARTESIAN_POINT ( 'NONE',  ( 0.3106000600989309857, -5.537975084925943037, -0.4079457818577079120 ) ) ;
#4467 = AXIS2_PLACEMENT_3D ( 'NONE', #5849, #7984, #12196 ) ;
#4468 = ORIENTED_EDGE ( 'NONE', *, *, #4827, .T. ) ;
#4469 = ADVANCED_FACE ( 'NONE', ( #4822 ), #10209, .T. ) ;
#4470 = VERTEX_POINT ( 'NONE', #3850 ) ;
#4471 = CARTESIAN_POINT ( 'NONE',  ( 4.132952817037860882, 4.063368025374523462, 1.253603594387587993E-15 ) ) ;
#4472 = EDGE_CURVE ( 'NONE', #2163, #7440, #3649, .T. ) ;
#4473 = CARTESIAN_POINT ( 'NONE',  ( 0.01055556052338869899, -4.084588180558399451, 2.925285743277528105 ) ) ;
#4474 =( NAMED_UNIT ( * ) SI_UNIT ( $, .STERADIAN. ) SOLID_ANGLE_UNIT ( ) );
#4475 = DIRECTION ( 'NONE',  ( 0.000000000000000000, 0.000000000000000000, 1.000000000000000000 ) ) ;
#4476 = DIRECTION ( 'NONE',  ( 0.000000000000000000, 0.000000000000000000, 1.000000000000000000 ) ) ;
#4477 = CARTESIAN_POINT ( 'NONE',  ( 52.29715082351547295, 52.39948385550240317, 6.992620115222774047 ) ) ;
#4478 = AXIS2_PLACEMENT_3D ( 'NONE', #10451, #11281, #8251 ) ;
#4479 = CARTESIAN_POINT ( 'NONE',  ( 54.13287192849671214, 56.70051614449766220, -5.649768623646139964 ) ) ;
#4480 = DIRECTION ( 'NONE',  ( 0.000000000000000000, 1.000000000000000000, 0.000000000000000000 ) ) ;
#4481 = CARTESIAN_POINT ( 'NONE',  ( 54.13287192849676188, 52.29948385550240886, 5.649768623646098220 ) ) ;
#4482 =( LENGTH_UNIT ( ) NAMED_UNIT ( * ) SI_UNIT ( .MILLI., .METRE. ) );
#4483 = VECTOR ( 'NONE', #6192, 1000.000000000000000 ) ;
#4484 = CARTESIAN_POINT ( 'NONE',  ( 56.81924384183011512, 62.19948385550240744, 4.924951120819313743 ) ) ;
#4485 = ORIENTED_EDGE ( 'NONE', *, *, #11334, .F. ) ;
#4486 = ORIENTED_EDGE ( 'NONE', *, *, #5120, .T. ) ;
#4487 = ORIENTED_EDGE ( 'NONE', *, *, #5916, .T. ) ;
#4488 = DIRECTION ( 'NONE',  ( -0.000000000000000000, -0.000000000000000000, -1.000000000000000000 ) ) ;
#4489 = EDGE_CURVE ( 'NONE', #4052, #2018, #10031, .T. ) ;
#4490 = DIRECTION ( 'NONE',  ( -1.000000000000000000, -0.000000000000000000, -0.000000000000000000 ) ) ;
#4491 = CARTESIAN_POINT ( 'NONE',  ( 55.69932041026405045, 55.10051614449765367, 1.875703265242156359 ) ) ;
#4492 = CARTESIAN_POINT ( 'NONE',  ( 7.547063560035813063E-16, -3.202582148906732762, -1.452965002680431272 ) ) ;
#4493 = CARTESIAN_POINT ( 'NONE',  ( 54.68390685589033495, 51.69948385550241454, -6.485486291978119766 ) ) ;
#4494 = CARTESIAN_POINT ( 'NONE',  ( 56.66441430157296821, 58.09948385550240602, 2.141517661632100111 ) ) ;
#4495 = CARTESIAN_POINT ( 'NONE',  ( 4.158921614371307918, 4.076055977742304215, -0.05993604794450364120 ) ) ;
#4496 = CARTESIAN_POINT ( 'NONE',  ( 54.72065718078924590, 46.29948385550240886, 6.458785618021043895 ) ) ;
#4497 = ORIENTED_EDGE ( 'NONE', *, *, #10943, .T. ) ;
#4498 = ADVANCED_FACE ( 'NONE', ( #10137 ), #2815, .F. ) ;
#4499 = ORIENTED_EDGE ( 'NONE', *, *, #7118, .F. ) ;
#4500 = EDGE_CURVE ( 'NONE', #2907, #178, #2671, .T. ) ;
#4501 = ORIENTED_EDGE ( 'NONE', *, *, #8150, .T. ) ;
#4502 = EDGE_LOOP ( 'NONE', ( #13380, #7746, #3956, #11568, #809, #6852 ) ) ;
#4503 = SHAPE_REPRESENTATION ( 'spring', ( #430 ), #3304 ) ;
#4504 = CARTESIAN_POINT ( 'NONE',  ( 62.49999999999998579, 40.00000000000001421, 5.000000000000000000 ) ) ;
#4505 = DIRECTION ( 'NONE',  ( -1.000000000000000000, 0.000000000000000000, 0.000000000000000000 ) ) ;
#4506 = EDGE_CURVE ( 'NONE', #1558, #6264, #1414, .T. ) ;
#4507 = CONICAL_SURFACE ( 'NONE', #1394, 4.000000000000003553, 1.029744260000001077 ) ;
#4508 = DIRECTION ( 'NONE',  ( 1.000000000000000000, 0.000000000000000000, 0.000000000000000000 ) ) ;
#4509 = CARTESIAN_POINT ( 'NONE',  ( 0.6507732100473444525, -4.243078065514795050, -0.2236248678334952777 ) ) ;
#4510 = CARTESIAN_POINT ( 'NONE',  ( 55.11794222512601493, 58.19948385550240744, 3.688883143319541702 ) ) ;
#4511 = CARTESIAN_POINT ( 'NONE',  ( 54.89903213687075834, 44.74560054925188268, -5.000000000000007105 ) ) ;
#4512 = VECTOR ( 'NONE', #6814, 1000.000000000000000 ) ;
#4513 = CARTESIAN_POINT ( 'NONE',  ( 56.79116909180259398, 55.20051614449766220, 4.963592699178938972 ) ) ;
#4514 =( REPRESENTATION_RELATIONSHIP ('NONE','NONE', #5328, #10956 ) REPRESENTATION_RELATIONSHIP_WITH_TRANSFORMATION ( #9294 )SHAPE_REPRESENTATION_RELATIONSHIP( ) );
#4515 = DIRECTION ( 'NONE',  ( -0.000000000000000000, -0.000000000000000000, -1.000000000000000000 ) ) ;
#4516 = DIRECTION ( 'NONE',  ( 0.000000000000000000, 0.000000000000000000, 1.000000000000000000 ) ) ;
#4517 = VECTOR ( 'NONE', #6446, 1000.000000000000000 ) ;
#4518 = CARTESIAN_POINT ( 'NONE',  ( 42.63976443033212860, 60.00051614449764514, -0.02388180880514948964 ) ) ;
#4519 = VECTOR ( 'NONE', #11952, 1000.000000000000000 ) ;
#4520 = ORIENTED_EDGE ( 'NONE', *, *, #10942, .T. ) ;
#4521 = LINE ( 'NONE', #10870, #8597 ) ;
#4522 = VECTOR ( 'NONE', #7105, 1000.000000000000227 ) ;
#4523 = VERTEX_POINT ( 'NONE', #12283 ) ;
#4524 = DIRECTION ( 'NONE',  ( 0.000000000000000000, 0.000000000000000000, 1.000000000000000000 ) ) ;
#4525 = CARTESIAN_POINT ( 'NONE',  ( 62.49999999999998579, 5.000000000000018652, -5.000000000000000000 ) ) ;
#4526 = DIRECTION ( 'NONE',  ( -1.000000000000000000, 0.000000000000000000, 0.000000000000000000 ) ) ;
#4527 =( NAMED_UNIT ( * ) SI_UNIT ( $, .STERADIAN. ) SOLID_ANGLE_UNIT ( ) );
#4528 = CARTESIAN_POINT ( 'NONE',  ( 52.25172492374522903, 59.59948385550240602, -7.007379884777225953 ) ) ;
#4529 = CONICAL_SURFACE ( 'NONE', #6318, 3.500000000000000000, 1.047197551196600296 ) ;
#4530 = CYLINDRICAL_SURFACE ( 'NONE', #431, 0.7500000000000000000 ) ;
#4531 = CARTESIAN_POINT ( 'NONE',  ( 55.11794222512599362, 60.80051614449766362, -3.688883143319583446 ) ) ;
#4532 = CARTESIAN_POINT ( 'NONE',  ( 6.165086708099361879, -6.325508935188243420, 0.000000000000000000 ) ) ;
#4533 = CARTESIAN_POINT ( 'NONE',  ( 0.4465819873852006072, 2.886751345948123770, -5.000000000000000000 ) ) ;
#4534 = CARTESIAN_POINT ( 'NONE',  ( 49.97728705011488159, 65.49948385550240459, -7.000000000000000888 ) ) ;
#4535 = CARTESIAN_POINT ( 'NONE',  ( 45.90387839640214196, 64.69948385550240744, 5.676469297603166098 ) ) ;
#4536 = CARTESIAN_POINT ( 'NONE',  ( -7.092489211676000613E-16, -4.452621892014641425, -2.287832656137186671 ) ) ;
#4537 = EDGE_LOOP ( 'NONE', ( #13176, #3606, #8862, #7020 ) ) ;
#4538 = VERTEX_POINT ( 'NONE', #3917 ) ;
#4539 = UNCERTAINTY_MEASURE_WITH_UNIT (LENGTH_MEASURE( 1.000000000000000082E-05 ), #10304, 'distance_accuracy_value', 'NONE');
#4540 = EDGE_CURVE ( 'NONE', #10018, #7328, #6900, .T. ) ;
#4541 = ORIENTED_EDGE ( 'NONE', *, *, #13352, .F. ) ;
#4542 = CARTESIAN_POINT ( 'NONE',  ( 2.354826896168714434, -6.962563485461402024, -1.000000000000000000 ) ) ;
#4543 = FACE_OUTER_BOUND ( 'NONE', #8308, .T. ) ;
#4544 = CARTESIAN_POINT ( 'NONE',  ( 4.180345304246197990, -2.049116244671341569, 3.591763845239312136 ) ) ;
#4545 =( NAMED_UNIT ( * ) PLANE_ANGLE_UNIT ( ) SI_UNIT ( $, .RADIAN. ) );
#4546 = CYLINDRICAL_SURFACE ( 'NONE', #3803, 9.999999999999998224 ) ;
#4547 = CARTESIAN_POINT ( 'NONE',  ( 4.154306624731137099, 2.398490048084935822, -3.721999068284414847 ) ) ;
#4548 = CARTESIAN_POINT ( 'NONE',  ( 57.36023556966787851, 49.99948385550239749, -0.02388180880522424582 ) ) ;
#4549 = CARTESIAN_POINT ( 'NONE',  ( 45.90387839640208512, 52.30051614449766362, -5.676469297603124353 ) ) ;
#4550 = DIRECTION ( 'NONE',  ( 0.000000000000000000, 0.000000000000000000, 1.000000000000000000 ) ) ;
#4551 = CARTESIAN_POINT ( 'NONE',  ( 49.97728705011488159, 53.49948385550240459, -7.000000000000000888 ) ) ;
#4552 = CARTESIAN_POINT ( 'NONE',  ( 44.03140696652192787, 47.19948385550240744, -4.306917132069425058 ) ) ;
#4553 = AXIS2_PLACEMENT_3D ( 'NONE', #920, #12477, #11587 ) ;
#4554 = CARTESIAN_POINT ( 'NONE',  ( 52.25172492374522903, 45.59948385550240602, -7.007379884777225953 ) ) ;
#4555 = VERTEX_POINT ( 'NONE', #6085 ) ;
#4556 = ORIENTED_EDGE ( 'NONE', *, *, #9097, .T. ) ;
#4557 = DIRECTION ( 'NONE',  ( 1.000000000000000000, 0.000000000000000000, 0.000000000000000000 ) ) ;
#4558 = EDGE_LOOP ( 'NONE', ( #12424, #7520, #10524, #12788 ) ) ;
#4559 = DIRECTION ( 'NONE',  ( -9.858538378746663627E-23, 5.031452844637890958E-23, -1.000000000000000000 ) ) ;
#4560 = CARTESIAN_POINT ( 'NONE',  ( -8.759913291900392807, -32.17636723815387256, 0.000000000000000000 ) ) ;
#4561 = VECTOR ( 'NONE', #749, 1000.000000000000000 ) ;
#4562 = CARTESIAN_POINT ( 'NONE',  ( 49.97728705011494554, 53.50051614449767357, 6.000000000000000888 ) ) ;
#4563 = CARTESIAN_POINT ( 'NONE',  ( -12.99038105676654453, -27.50000000000006040, 9.000000000000000000 ) ) ;
#4564 = CARTESIAN_POINT ( 'NONE',  ( 56.79116909180255135, 51.79948385550240175, -4.963592699179005585 ) ) ;
#4565 = CARTESIAN_POINT ( 'NONE',  ( 55.96859303347804371, 54.19948385550240033, 4.306917132069425946 ) ) ;
#4566 = DIRECTION ( 'NONE',  ( 0.000000000000000000, -0.4999999999999991118, 0.8660254037844391517 ) ) ;
#4567 = EDGE_CURVE ( 'NONE', #8675, #4780, #7871, .T. ) ;
#4568 = CARTESIAN_POINT ( 'NONE',  ( 54.68390685589039890, 61.30051614449766362, 6.485486291978072693 ) ) ;
#4569 = PRODUCT_DEFINITION_SHAPE ( 'NONE', 'NONE',  #13666 ) ;
#4570 = EDGE_LOOP ( 'NONE', ( #9375, #6850, #3804 ) ) ;
#4571 = VERTEX_POINT ( 'NONE', #4690 ) ;
#4572 = EDGE_LOOP ( 'NONE', ( #6523, #2211, #10972, #11094 ) ) ;
#4573 = VERTEX_POINT ( 'NONE', #8143 ) ;
#4574 = DIRECTION ( 'NONE',  ( -1.000000000000000000, 0.000000000000000000, 0.000000000000000000 ) ) ;
#4575 = DIRECTION ( 'NONE',  ( -0.000000000000000000, 0.000000000000000000, -1.000000000000000000 ) ) ;
#4576 = EDGE_CURVE ( 'NONE', #8730, #2436, #11033, .T. ) ;
#4577 = DIRECTION ( 'NONE',  ( 0.000000000000000000, 0.000000000000000000, -1.000000000000000000 ) ) ;
#4578 = B_SPLINE_CURVE_WITH_KNOTS ( 'NONE', 3,
 ( #6916, #10015, #532, #8988, #10981 ),
 .UNSPECIFIED., .F., .F.,
 ( 4, 1, 4 ),
 ( 0.000000000000000000, 0.002886751345948128985, 0.005773502691896257970 ),
 .UNSPECIFIED. ) ;
#4579 = FACE_OUTER_BOUND ( 'NONE', #1576, .T. ) ;
#4580 = CARTESIAN_POINT ( 'NONE',  ( 50.02271294988511841, 56.49948385550240459, 6.000000000000000888 ) ) ;
#4581 = CARTESIAN_POINT ( 'NONE',  ( 47.74827507625470702, 46.40051614449765083, -7.007379884777204637 ) ) ;
#4582 = EDGE_CURVE ( 'NONE', #11747, #13619, #2599, .T. ) ;
#4583 = CARTESIAN_POINT ( 'NONE',  ( 47.42335538002180328, 50.40051614449766504, -8.007379884777206414 ) ) ;
#4584 = EDGE_CURVE ( 'NONE', #13041, #2414, #3203, .T. ) ;
#4585 = CARTESIAN_POINT ( 'NONE',  ( 2.000000000000000000, -6.429618962271402616, 0.000000000000000000 ) ) ;
#4586 = CARTESIAN_POINT ( 'NONE',  ( 1.567478505476134606E-15, 4.618802153517012066, -5.000000000000000000 ) ) ;
#4587 = CARTESIAN_POINT ( 'NONE',  ( 47.74827507625469281, 64.40051614449765793, -7.007379884777203749 ) ) ;
#4588 = ORIENTED_EDGE ( 'NONE', *, *, #3729, .T. ) ;
#4589 = DIRECTION ( 'NONE',  ( 1.000000000000000000, 0.000000000000000000, 0.000000000000000000 ) ) ;
#4590 = B_SPLINE_CURVE_WITH_KNOTS ( 'NONE', 3,
 ( #12873, #13262, #2772, #2367, #3553 ),
 .UNSPECIFIED., .F., .F.,
 ( 4, 1, 4 ),
 ( 0.000000000000000000, 0.002886751345948122913, 0.005773502691896245827 ),
 .UNSPECIFIED. ) ;
#4591 = ORIENTED_EDGE ( 'NONE', *, *, #9959, .T. ) ;
#4592 = DIRECTION ( 'NONE',  ( -1.000000000000000000, 0.000000000000000000, 0.000000000000000000 ) ) ;
#4593 = CARTESIAN_POINT ( 'NONE',  ( 2.449293598294706513E-15, -20.00000000000000000, -9.999999999999994671 ) ) ;
#4594 = CARTESIAN_POINT ( 'NONE',  ( 3.948103430090710297, -3.379418997638724331, -1.146674596026246551 ) ) ;
#4595 = DIRECTION ( 'NONE',  ( 0.000000000000000000, 0.000000000000000000, -1.000000000000000000 ) ) ;
#4596 = CARTESIAN_POINT ( 'NONE',  ( 54.13287192849676188, 60.29948385550240886, 5.649768623646098220 ) ) ;
#4597 =( GEOMETRIC_REPRESENTATION_CONTEXT ( 3 ) GLOBAL_UNCERTAINTY_ASSIGNED_CONTEXT ( ( #13412 ) ) GLOBAL_UNIT_ASSIGNED_CONTEXT ( ( #11899, #5424, #4646 ) ) REPRESENTATION_CONTEXT ( 'NONE', 'WORKASPACE' ) );
#4598 = EDGE_CURVE ( 'NONE', #7759, #3701, #11804, .T. ) ;
#4599 = EDGE_CURVE ( 'NONE', #13259, #11359, #13168, .T. ) ;
#4600 = CARTESIAN_POINT ( 'NONE',  ( 55.71335778527780036, 58.90051614449766504, -1.832500667257213056 ) ) ;
#4601 = CARTESIAN_POINT ( 'NONE',  ( 2.449293598294706513E-15, -20.00000000000000000, -8.999999999999998224 ) ) ;
#4602 = DIRECTION ( 'NONE',  ( 0.000000000000000000, 0.000000000000000000, 1.000000000000000000 ) ) ;
#4603 = CARTESIAN_POINT ( 'NONE',  ( 43.34962307344078880, 46.10051614449766078, -2.184720259617096705 ) ) ;
#4604 = CARTESIAN_POINT ( 'NONE',  ( 51.92680522751233951, 47.59948385550239891, -6.007379884777223289 ) ) ;
#4605 = FACE_OUTER_BOUND ( 'NONE', #1032, .T. ) ;
#4606 = VERTEX_POINT ( 'NONE', #12148 ) ;
#4607 = EDGE_LOOP ( 'NONE', ( #10427, #7252, #9828, #293 ) ) ;
#4608 = CIRCLE ( 'NONE', #12767, 3.500000000000000000 ) ;
#4609 = ORIENTED_EDGE ( 'NONE', *, *, #9240, .T. ) ;
#4610 = DIRECTION ( 'NONE',  ( -1.000000000000000000, 0.000000000000000000, 0.000000000000000000 ) ) ;
#4611 = AXIS2_PLACEMENT_3D ( 'NONE', #9446, #11451, #10412 ) ;
#4612 = CARTESIAN_POINT ( 'NONE',  ( 4.236525694536557474, -2.416953475386482530, -3.751298745799839462 ) ) ;
#4613 = CARTESIAN_POINT ( 'NONE',  ( 4.630153689607048761, 6.577590292450083844E-16, 5.371010071662833063 ) ) ;
#4614 =( LENGTH_UNIT ( ) NAMED_UNIT ( * ) SI_UNIT ( .MILLI., .METRE. ) );
#4615 = LINE ( 'NONE', #13163, #13068 ) ;
#4616 = CARTESIAN_POINT ( 'NONE',  ( 4.071447262713887127, -2.020725942163686284, 3.500000000000000444 ) ) ;
#4617 = EDGE_CURVE ( 'NONE', #65, #13462, #11973, .T. ) ;
#4618 = CARTESIAN_POINT ( 'NONE',  ( 55.94051828345053679, 53.20051614449766220, 4.345558710429044069 ) ) ;
#4619 = AXIS2_PLACEMENT_3D ( 'NONE', #5305, #13640, #6541 ) ;
#4620 = EDGE_CURVE ( 'NONE', #10162, #6905, #576, .T. ) ;
#4621 = DIRECTION ( 'NONE',  ( -4.082155997157844188E-16, 1.000000000000000000, 0.000000000000000000 ) ) ;
#4622 = CARTESIAN_POINT ( 'NONE',  ( 52.25172492374522903, 51.59948385550240602, -7.007379884777225953 ) ) ;
#4623 = CIRCLE ( 'NONE', #848, 15.00000000000000000 ) ;
#4624 = CARTESIAN_POINT ( 'NONE',  ( 55.96859303347804371, 48.19948385550240033, 4.306917132069425946 ) ) ;
#4625 = CARTESIAN_POINT ( 'NONE',  ( 42.39856655714566358, 60.89948385550241028, 2.493737253992119207 ) ) ;
#4626 = ORIENTED_EDGE ( 'NONE', *, *, #9234, .T. ) ;
#4627 = ORIENTED_EDGE ( 'NONE', *, *, #9584, .T. ) ;
#4628 = COLOUR_RGB ( '',1.000000000000000000, 0.9490196078431372140, 0.9098039215686274384 ) ;
#4629 = CARTESIAN_POINT ( 'NONE',  ( 3.958476099524539382, -1.406653531810738933, -3.499999999999999556 ) ) ;
#4630 = EDGE_LOOP ( 'NONE', ( #11496, #11421, #3010, #12787, #7893, #9131, #10354 ) ) ;
#4631 = FACE_OUTER_BOUND ( 'NONE', #2905, .T. ) ;
#4632 = CARTESIAN_POINT ( 'NONE',  ( 2.000000000000000000, 1.773042676681340524, -2.059984127722458425E-15 ) ) ;
#4633 = CARTESIAN_POINT ( 'NONE',  ( 44.88205777487401349, 53.80051614449766362, 3.688883143319584779 ) ) ;
#4634 = CARTESIAN_POINT ( 'NONE',  ( -7.499999999999923617, -32.99038105676662269, 9.000000000000000000 ) ) ;
#4635 = CARTESIAN_POINT ( 'NONE',  ( 45.31609314410967926, 52.69948385550240744, 6.485486291978119766 ) ) ;
#4636 = CARTESIAN_POINT ( 'NONE',  ( 55.94051828345050836, 57.79948385550238754, -4.345558710429104465 ) ) ;
#4637 = CARTESIAN_POINT ( 'NONE',  ( 4.082498951862920222, -4.041451884327386779, 0.000000000000000000 ) ) ;
#4638 = CARTESIAN_POINT ( 'NONE',  ( 54.72065718078918906, 62.70051614449766220, -6.458785618021089192 ) ) ;
#4640 = EDGE_CURVE ( 'NONE', #8508, #5565, #8005, .T. ) ;
#4639 = ORIENTED_EDGE ( 'NONE', *, *, #11441, .T. ) ;
#4641 = ITEM_DEFINED_TRANSFORMATION ( 'NONE', 'NONE', #12141,  #430 ) ;
#4642 = ORIENTED_EDGE ( 'NONE', *, *, #4715, .T. ) ;
#4643 = VERTEX_POINT ( 'NONE', #8486 ) ;
#4644 = ORIENTED_EDGE ( 'NONE', *, *, #52, .T. ) ;
#4645 = CARTESIAN_POINT ( 'NONE',  ( 6.270568613849413886, 3.932080789230360196, -3.401571648088637101 ) ) ;
#4646 =( NAMED_UNIT ( * ) SI_UNIT ( $, .STERADIAN. ) SOLID_ANGLE_UNIT ( ) );
#4647 = EDGE_CURVE ( 'NONE', #5390, #10855, #9672, .T. ) ;
#4648 = LINE ( 'NONE', #2353, #7962 ) ;
#4649 = DIRECTION ( 'NONE',  ( -0.000000000000000000, -0.000000000000000000, 1.000000000000000000 ) ) ;
#4650 = CARTESIAN_POINT ( 'NONE',  ( 56.30877334542961421, 53.99948385550241170, -0.02388180880520959434 ) ) ;
#4651 = CARTESIAN_POINT ( 'NONE',  ( 56.65037692655921120, 47.10051614449766078, 2.184720259617097593 ) ) ;
#4652 = CARTESIAN_POINT ( 'NONE',  ( 43.18075615816994173, 53.80051614449766362, 4.924951120819380357 ) ) ;
#4653 = CYLINDRICAL_SURFACE ( 'NONE', #13272, 2.149999999999999023 ) ;
#4654 = CARTESIAN_POINT ( 'NONE',  ( 52.60990417590917900, 44.99999999999999289, -5.983956152663589378 ) ) ;
#4655 = CARTESIAN_POINT ( 'NONE',  ( 42.63976443033212860, 64.00051614449765225, -0.02388180880514948964 ) ) ;
#4656 = CIRCLE ( 'NONE', #5770, 2.649999999999987477 ) ;
#4657 = VERTEX_POINT ( 'NONE', #13440 ) ;
#4658 = CARTESIAN_POINT ( 'NONE',  ( -0.6937372685066653943, 4.453844082567723461, -3.610536846335889116 ) ) ;
#4659 = VERTEX_POINT ( 'NONE', #998 ) ;
#4660 = EDGE_CURVE ( 'NONE', #7376, #3807, #10485, .T. ) ;
#4661 = CARTESIAN_POINT ( 'NONE',  ( -62.49999999999997158, 40.00000000000001421, 9.999999999999998224 ) ) ;
#4662 = CARTESIAN_POINT ( 'NONE',  ( 4.175813232069147674, 2.061359961916367833, 3.570380186727398097 ) ) ;
#4663 = AXIS2_PLACEMENT_3D ( 'NONE', #12635, #250, #10560 ) ;
#4664 = CARTESIAN_POINT ( 'NONE',  ( 0.000000000000000000, 15.00000000000001599, 20.60000000000000142 ) ) ;
#4665 = CARTESIAN_POINT ( 'NONE',  ( 52.29715082351547295, 54.39948385550239607, 6.992620115222774047 ) ) ;
#4666 = CARTESIAN_POINT ( 'NONE',  ( 46.45491332379576477, 59.70051614449766220, 4.840751629271188961 ) ) ;
#4667 = CARTESIAN_POINT ( 'NONE',  ( 4.050823680195224874, -2.400527758044906701, -2.978030508226146900 ) ) ;
#4668 = CARTESIAN_POINT ( 'NONE',  ( -12.99038105676659427, -12.50000000000003020, -9.000000000000000000 ) ) ;
#4669 = CARTESIAN_POINT ( 'NONE',  ( 44.28664221472221385, 63.90051614449765793, 1.832500667257213722 ) ) ;
#4670 = CARTESIAN_POINT ( 'NONE',  ( 55.69932041026404335, 45.89948385550240317, -1.875703265242203432 ) ) ;
#4671 = PLANE ( 'NONE',  #13117 ) ;
#4672 = EDGE_LOOP ( 'NONE', ( #5205, #6815, #8789 ) ) ;
#4673 = CIRCLE ( 'NONE', #9096, 0.7499999999999997780 ) ;
#4674 = CIRCLE ( 'NONE', #2236, 2.500000000000000444 ) ;
#4675 = UNCERTAINTY_MEASURE_WITH_UNIT (LENGTH_MEASURE( 1.000000000000000082E-05 ), #9384, 'distance_accuracy_value', 'NONE');
#4677 = EDGE_CURVE ( 'NONE', #5173, #10123, #3418, .T. ) ;
#4676 = ORIENTED_EDGE ( 'NONE', *, *, #1021, .F. ) ;
#4678 = CARTESIAN_POINT ( 'NONE',  ( 0.000000000000000000, 0.000000000000000000, 15.00000000000000000 ) ) ;
#4679 = ADVANCED_FACE ( 'NONE', ( #10415, #7451 ), #11655, .F. ) ;
#4680 = CARTESIAN_POINT ( 'NONE',  ( 4.207491450040567571, -2.029819825146485179, -3.671670828759567407 ) ) ;
#4681 = CYLINDRICAL_SURFACE ( 'NONE', #10187, 1.500000000000001332 ) ;
#4682 = SURFACE_STYLE_USAGE ( .BOTH. , #2666 ) ;
#4683 = DIRECTION ( 'NONE',  ( 1.000000000000000000, 3.469446951953615175E-16, 0.000000000000000000 ) ) ;
#4684 = EDGE_CURVE ( 'NONE', #7378, #11021, #1979, .T. ) ;
#4685 = PLANE ( 'NONE',  #7346 ) ;
#4686 = AXIS2_PLACEMENT_3D ( 'NONE', #8339, #12471, #13494 ) ;
#4687 = CARTESIAN_POINT ( 'NONE',  ( 55.96859303347802239, 50.80051614449766362, -4.306917132069484566 ) ) ;
#4688 = CARTESIAN_POINT ( 'NONE',  ( 14.92499999999998650, -18.50187617334198009, 0.000000000000000000 ) ) ;
#4689 = CIRCLE ( 'NONE', #2919, 7.500000000000000888 ) ;
#4690 = CARTESIAN_POINT ( 'NONE',  ( 45.60000000000000142, 0.000000000000000000, 2.055000000000000160 ) ) ;
#4691 = CARTESIAN_POINT ( 'NONE',  ( 42.63976443033212860, 54.99948385550241170, 0.02388180880522514787 ) ) ;
#4692 = CARTESIAN_POINT ( 'NONE',  ( 55.96859303347804371, 46.19948385550238612, 4.306917132069425946 ) ) ;
#4693 = CARTESIAN_POINT ( 'NONE',  ( 43.20883090819745576, 60.79948385550241596, 4.963592699179006473 ) ) ;
#4694 = ORIENTED_EDGE ( 'NONE', *, *, #623, .T. ) ;
#4695 = VERTEX_POINT ( 'NONE', #9390 ) ;
#4696 = CARTESIAN_POINT ( 'NONE',  ( 0.000000000000000000, 4.898587196589412829E-16, -4.000000000000000000 ) ) ;
#4697 = AXIS2_PLACEMENT_3D ( 'NONE', #7929, #511, #1617 ) ;
#4698 = ORIENTED_EDGE ( 'NONE', *, *, #341, .F. ) ;
#4699 = DIRECTION ( 'NONE',  ( -1.000000000000000000, -0.000000000000000000, -0.000000000000000000 ) ) ;
#4700 =( REPRESENTATION_RELATIONSHIP ('NONE','NONE', #5328, #11930 ) REPRESENTATION_RELATIONSHIP_WITH_TRANSFORMATION ( #1575 )SHAPE_REPRESENTATION_RELATIONSHIP( ) );
#4701 = VECTOR ( 'NONE', #3546, 1000.000000000000000 ) ;
#4702 = CYLINDRICAL_SURFACE ( 'NONE', #12782, 2.396904916527699214 ) ;
#4703 = CARTESIAN_POINT ( 'NONE',  ( 46.45491332379576477, 55.70051614449766220, 4.840751629271188961 ) ) ;
#4704 = DIRECTION ( 'NONE',  ( -0.000000000000000000, -0.000000000000000000, 1.000000000000000000 ) ) ;
#4705 = CARTESIAN_POINT ( 'NONE',  ( 45.27934281921075410, 51.29948385550240175, -6.458785618021043895 ) ) ;
#4706 = EDGE_CURVE ( 'NONE', #408, #9920, #10919, .T. ) ;
#4707 = CARTESIAN_POINT ( 'NONE',  ( 45.90387839640214196, 58.69948385550240033, 5.676469297603166098 ) ) ;
#4708 = CARTESIAN_POINT ( 'NONE',  ( 4.093692494532774617, -4.043567292011547742, 3.285329657490527105E-16 ) ) ;
#4709 = CARTESIAN_POINT ( 'NONE',  ( 56.79116909180255135, 45.79948385550240886, -4.963592699179005585 ) ) ;
#4710 = VECTOR ( 'NONE', #4566, 1000.000000000000000 ) ;
#4711 = ORIENTED_EDGE ( 'NONE', *, *, #1519, .F. ) ;
#4712 = VERTEX_POINT ( 'NONE', #8422 ) ;
#4713 = ORIENTED_EDGE ( 'NONE', *, *, #11474, .T. ) ;
#4714 = ORIENTED_EDGE ( 'NONE', *, *, #12713, .T. ) ;
#4715 = EDGE_CURVE ( 'NONE', #12675, #1912, #5137, .T. ) ;
#4716 = AXIS2_PLACEMENT_3D ( 'NONE', #8140, #2953, #7029 ) ;
#4717 = DIRECTION ( 'NONE',  ( -1.000000000000000000, 1.734723475976806848E-16, 0.000000000000000000 ) ) ;
#4718 = DIRECTION ( 'NONE',  ( -0.000000000000000000, -0.000000000000000000, 1.000000000000000000 ) ) ;
#4719 = DIRECTION ( 'NONE',  ( -4.082155997157844188E-16, 1.000000000000000000, 0.000000000000000000 ) ) ;
#4720 = CARTESIAN_POINT ( 'NONE',  ( 48.02776887271745210, 55.39948385550240317, -5.992620115222778487 ) ) ;
#4721 = CARTESIAN_POINT ( 'NONE',  ( 52.29715082351539479, 46.60051614449766078, -6.992620115222796251 ) ) ;
#4722 = CARTESIAN_POINT ( 'NONE',  ( 58.41169779390614281, 53.00051614449765935, 0.02388180880515032231 ) ) ;
#4723 = ADVANCED_FACE ( 'NONE', ( #7180 ), #322, .T. ) ;
#4724 = FACE_OUTER_BOUND ( 'NONE', #8254, .T. ) ;
#4725 = FACE_OUTER_BOUND ( 'NONE', #4450, .T. ) ;
#4726 = CARTESIAN_POINT ( 'NONE',  ( 56.79116909180259398, 45.20051614449766220, 4.963592699178938972 ) ) ;
#4727 = PRODUCT_DEFINITION ( 'UNKNOWN', '', #3313, #2318 ) ;
#4728 = ORIENTED_EDGE ( 'NONE', *, *, #5120, .F. ) ;
#4729 = CARTESIAN_POINT ( 'NONE',  ( 4.175813232069148562, -2.061359961916374051, -3.570380186727397653 ) ) ;
#4730 = AXIS2_PLACEMENT_3D ( 'NONE', #6820, #1614, #2592 ) ;
#4731 = ORIENTED_EDGE ( 'NONE', *, *, #12070, .T. ) ;
#4732 = FACE_OUTER_BOUND ( 'NONE', #10721, .T. ) ;
#4733 = CARTESIAN_POINT ( 'NONE',  ( 4.033901012035484790, -2.321269032827465661, -2.979444097106959788 ) ) ;
#4734 = DIRECTION ( 'NONE',  ( 1.000000000000000000, 0.000000000000000000, 0.000000000000000000 ) ) ;
#4735 = CARTESIAN_POINT ( 'NONE',  ( 44.05948171654949874, 56.79948385550240886, 4.345558710429105354 ) ) ;
#4736 = CARTESIAN_POINT ( 'NONE',  ( 44.30067958973594955, 58.10051614449765367, -1.875703265242155693 ) ) ;
#4737 = CONICAL_SURFACE ( 'NONE', #303, 5.000000000000000000, 1.047197551196600296 ) ;
#4738 = CARTESIAN_POINT ( 'NONE',  ( 2.449293598294706513E-15, -5.000000000000000888, -9.000000000000000000 ) ) ;
#4739 = DIRECTION ( 'NONE',  ( -1.000000000000000000, 0.000000000000000000, 0.000000000000000000 ) ) ;
#4740 = CARTESIAN_POINT ( 'NONE',  ( 54.09612160359792199, 47.30051614449765651, 5.676469297603124353 ) ) ;
#4741 = CARTESIAN_POINT ( 'NONE',  ( 53.54508667620428497, 48.29948385550240175, 4.840751629271157874 ) ) ;
#4742 = DIRECTION ( 'NONE',  ( -1.000000000000000000, -0.000000000000000000, -0.000000000000000000 ) ) ;
#4743 = EDGE_LOOP ( 'NONE', ( #6316, #9826, #7860, #3569 ) ) ;
#4744 = AXIS2_PLACEMENT_3D ( 'NONE', #9654, #1262, #5513 ) ;
#4745 = ADVANCED_FACE ( 'NONE', ( #3989 ), #5109, .T. ) ;
#4746 = ORIENTED_EDGE ( 'NONE', *, *, #8633, .T. ) ;
#4747 = CARTESIAN_POINT ( 'NONE',  ( 0.4465819873849485311, -2.886751345948517677, -5.000000000000000000 ) ) ;
#4748 = CIRCLE ( 'NONE', #5202, 1.999999999999998224 ) ;
#4749 = CARTESIAN_POINT ( 'NONE',  ( 2.345747346278113987, -3.264484291692503870, -0.01223254789874484924 ) ) ;
#4750 = CARTESIAN_POINT ( 'NONE',  ( 0.8816464618332836567, -24.71833652004169934, 9.999999999999998224 ) ) ;
#4751 =( LENGTH_UNIT ( ) NAMED_UNIT ( * ) SI_UNIT ( .MILLI., .METRE. ) );
#4752 = CARTESIAN_POINT ( 'NONE',  ( -12.50000000000000000, 15.00000000000001599, -9.000000000000000000 ) ) ;
#4753 = CARTESIAN_POINT ( 'NONE',  ( -2.500000000000000444, 3.061616997868383634E-16, -25.03750572909317285 ) ) ;
#4754 = EDGE_CURVE ( 'NONE', #5030, #10987, #2110, .T. ) ;
#4755 = CARTESIAN_POINT ( 'NONE',  ( 55.96859303347802239, 62.80051614449766362, -4.306917132069484566 ) ) ;
#4756 = DIRECTION ( 'NONE',  ( 1.000000000000000000, 0.000000000000000000, 0.000000000000000000 ) ) ;
#4757 = DIRECTION ( 'NONE',  ( 1.000000000000000000, -0.000000000000000000, 0.000000000000000000 ) ) ;
#4758 = CARTESIAN_POINT ( 'NONE',  ( 55.94051828345050836, 59.79948385550238754, -4.345558710429104465 ) ) ;
#4759 = EDGE_CURVE ( 'NONE', #7327, #2789, #8724, .T. ) ;
#4760 = CARTESIAN_POINT ( 'NONE',  ( 54.09612160359786515, 47.69948385550240744, -5.676469297603166098 ) ) ;
#4761 = EDGE_CURVE ( 'NONE', #1857, #2588, #3862, .T. ) ;
#4762 = CARTESIAN_POINT ( 'NONE',  ( 54.68390685589033495, 63.69948385550240033, -6.485486291978119766 ) ) ;
#4763 = ORIENTED_EDGE ( 'NONE', *, *, #11996, .F. ) ;
#4764 = ORIENTED_EDGE ( 'NONE', *, *, #11163, .T. ) ;
#4765 = DIRECTION ( 'NONE',  ( 1.000000000000000000, 0.000000000000000000, 0.000000000000000000 ) ) ;
#4766 = EDGE_CURVE ( 'NONE', #10184, #9080, #9318, .T. ) ;
#4767 = ORIENTED_EDGE ( 'NONE', *, *, #12758, .F. ) ;
#4768 = DIRECTION ( 'NONE',  ( -0.000000000000000000, -0.000000000000000000, 1.000000000000000000 ) ) ;
#4769 = CARTESIAN_POINT ( 'NONE',  ( 6.534838248920899595, -2.951765777552420644, -5.112608298763837489 ) ) ;
#4770 = CARTESIAN_POINT ( 'NONE',  ( 48.07319477248762496, 58.40051614449765793, -6.007379884777208190 ) ) ;
#4771 = CARTESIAN_POINT ( 'NONE',  ( -4.197393957002303999, 0.4069871074557429025, -3.503767560748926257 ) ) ;
#4772 = CARTESIAN_POINT ( 'NONE',  ( 43.20883090819745576, 54.79948385550240175, 4.963592699179006473 ) ) ;
#4773 = CARTESIAN_POINT ( 'NONE',  ( 47.74827507625478518, 54.59948385550239180, 7.007379884777227730 ) ) ;
#4774 = DIRECTION ( 'NONE',  ( 0.000000000000000000, 0.5150380737757248584, 0.8571673013836862420 ) ) ;
#4775 = CARTESIAN_POINT ( 'NONE',  ( 43.18075615816994173, 59.80051614449766362, 4.924951120819380357 ) ) ;
#4776 = ORIENTED_EDGE ( 'NONE', *, *, #928, .F. ) ;
#4777 = ORIENTED_EDGE ( 'NONE', *, *, #5591, .T. ) ;
#4778 = APPLICATION_CONTEXT ( 'automotive_design' ) ;
#4779 = CIRCLE ( 'NONE', #7434, 5.384454397937118664 ) ;
#4780 = VERTEX_POINT ( 'NONE', #7248 ) ;
#4781 = VERTEX_POINT ( 'NONE', #8214 ) ;
#4782 = AXIS2_PLACEMENT_3D ( 'NONE', #3677, #6998, #13401 ) ;
#4783 = CARTESIAN_POINT ( 'NONE',  ( 12.17636723815389566, -28.75991329190035373, 0.000000000000000000 ) ) ;
#4784 = LINE ( 'NONE', #13134, #4214 ) ;
#4785 = LINE ( 'NONE', #6111, #10430 ) ;
#4786 = DIRECTION ( 'NONE',  ( 1.000000000000000000, 0.000000000000000000, 0.000000000000000000 ) ) ;
#4787 = LINE ( 'NONE', #7066, #2796 ) ;
#4788 = CARTESIAN_POINT ( 'NONE',  ( 44.88205777487398507, 59.19948385550240744, -3.688883143319540814 ) ) ;
#4789 = CARTESIAN_POINT ( 'NONE',  ( 47.74827507625470702, 54.40051614449765793, -7.007379884777204637 ) ) ;
#4790 = CARTESIAN_POINT ( 'NONE',  ( 54.72065718078918906, 54.70051614449765509, -6.458785618021089192 ) ) ;
#4791 = EDGE_CURVE ( 'NONE', #11878, #11056, #5359, .T. ) ;
#4792 = CARTESIAN_POINT ( 'NONE',  ( 75.00000000000001421, -7.499999999999971578, -10.00000000000000000 ) ) ;
#4793 = DIRECTION ( 'NONE',  ( -1.000000000000000000, 0.000000000000000000, 0.000000000000000000 ) ) ;
#4794 = CARTESIAN_POINT ( 'NONE',  ( 54.13287192849671214, 62.70051614449766220, -5.649768623646139964 ) ) ;
#4795 = ORIENTED_EDGE ( 'NONE', *, *, #11342, .T. ) ;
#4796 = CARTESIAN_POINT ( 'NONE',  ( -2.688821387764050996E-14, -4.618802153517012954, -0.4999999999999995559 ) ) ;
#4797 = ORIENTED_EDGE ( 'NONE', *, *, #1991, .F. ) ;
#4798 = DIRECTION ( 'NONE',  ( 0.000000000000000000, 0.4999999999999989453, -0.8660254037844391517 ) ) ;
#4799 = DIRECTION ( 'NONE',  ( -0.7779254092217071648, -0.6283566325640553840, 0.000000000000000000 ) ) ;
#4800 = DIRECTION ( 'NONE',  ( 0.000000000000000000, 0.000000000000000000, -1.000000000000000000 ) ) ;
#4801 = CARTESIAN_POINT ( 'NONE',  ( 47.70284917648453415, 57.39948385550241028, -6.992620115222774047 ) ) ;
#4802 = CARTESIAN_POINT ( 'NONE',  ( 49.97728705011488159, 55.49948385550240459, -7.000000000000000888 ) ) ;
#4803 = B_SPLINE_CURVE_WITH_KNOTS ( 'NONE', 3,
 ( #13424, #9089, #7159, #7087, #1889 ),
 .UNSPECIFIED., .F., .F.,
 ( 4, 1, 4 ),
 ( 0.000000000000000000, 0.002309401076758505790, 0.004618802153517011580 ),
 .UNSPECIFIED. ) ;
#4804 = CARTESIAN_POINT ( 'NONE',  ( 0.1388410611046082266, -2.351840044243035166, 2.926493552096024242 ) ) ;
#4805 = CARTESIAN_POINT ( 'NONE',  ( 2.449293598294706513E-15, -20.00000000000000000, 15.00000000000000355 ) ) ;
#4806 = CARTESIAN_POINT ( 'NONE',  ( 2.000000000000000000, -0.8865213383406694847, 1.535500000000001419 ) ) ;
#4807 = CARTESIAN_POINT ( 'NONE',  ( 42.63976443033212860, 46.00051614449766646, -0.02388180880514948964 ) ) ;
#4808 = CARTESIAN_POINT ( 'NONE',  ( 55.94051828345050836, 63.79948385550240886, -4.345558710429104465 ) ) ;
#4809 = DIRECTION ( 'NONE',  ( -1.000000000000000000, 0.000000000000000000, 0.000000000000000000 ) ) ;
#4810 = VERTEX_POINT ( 'NONE', #4268 ) ;
#4811 = EDGE_CURVE ( 'NONE', #3296, #6833, #834, .T. ) ;
#4812 = VERTEX_POINT ( 'NONE', #2724 ) ;
#4813 = EDGE_LOOP ( 'NONE', ( #5808, #796, #4468, #11877 ) ) ;
#4814 = FACE_BOUND ( 'NONE', #9026, .T. ) ;
#4815 = CARTESIAN_POINT ( 'NONE',  ( 2.595115354961440524, -7.673029147243177306, -1.000000000000000000 ) ) ;
#4816 = CARTESIAN_POINT ( 'NONE',  ( 6.385552186430388133, -2.886751345948118441, 5.000000000000000888 ) ) ;
#4817 = CARTESIAN_POINT ( 'NONE',  ( -13.67449106481164733, -26.16508670809959725, 9.000000000000000000 ) ) ;
#4818 = CARTESIAN_POINT ( 'NONE',  ( 0.000000000000000000, 0.000000000000000000, 0.000000000000000000 ) ) ;
#4819 = EDGE_CURVE ( 'NONE', #10123, #5173, #9333, .T. ) ;
#4820 = CARTESIAN_POINT ( 'NONE',  ( 54.09612160359792199, 63.30051614449766362, 5.676469297603124353 ) ) ;
#4821 = DIRECTION ( 'NONE',  ( 0.000000000000000000, 0.000000000000000000, -1.000000000000000000 ) ) ;
#4822 = FACE_OUTER_BOUND ( 'NONE', #4958, .T. ) ;
#4823 = CARTESIAN_POINT ( 'NONE',  ( 47.74827507625478518, 56.59948385550238470, 7.007379884777227730 ) ) ;
#4824 = CARTESIAN_POINT ( 'NONE',  ( 47.74827507625478518, 46.59948385550239891, 7.007379884777227730 ) ) ;
#4825 = VECTOR ( 'NONE', #314, 1000.000000000000000 ) ;
#4826 = CARTESIAN_POINT ( 'NONE',  ( 54.13287192849676188, 46.29948385550240886, 5.649768623646098220 ) ) ;
#4827 = EDGE_CURVE ( 'NONE', #10268, #582, #9540, .T. ) ;
#4828 = ORIENTED_EDGE ( 'NONE', *, *, #9240, .F. ) ;
#4829 = ORIENTED_EDGE ( 'NONE', *, *, #12029, .T. ) ;
#4830 = CARTESIAN_POINT ( 'NONE',  ( 14.92499999999998650, -18.50187617334196943, -9.000000000000000000 ) ) ;
#4831 = ORIENTED_EDGE ( 'NONE', *, *, #3251, .T. ) ;
#4832 = EDGE_CURVE ( 'NONE', #11691, #1754, #10328, .T. ) ;
#4833 = CARTESIAN_POINT ( 'NONE',  ( 5.000000000000003553, -20.00000000000000000, 15.00000000000000355 ) ) ;
#4834 = EDGE_CURVE ( 'NONE', #9183, #10142, #12329, .T. ) ;
#4835 = VECTOR ( 'NONE', #2437, 1000.000000000000000 ) ;
#4836 = FACE_OUTER_BOUND ( 'NONE', #12255, .T. ) ;
#4837 = CONICAL_SURFACE ( 'NONE', #4611, 3.500000000000000000, 1.047197551196600296 ) ;
#4838 = CARTESIAN_POINT ( 'NONE',  ( 51.92680522751238925, 63.40051614449765083, 6.007379884777208190 ) ) ;
#4839 = CARTESIAN_POINT ( 'NONE',  ( 0.03027795056225670092, 0.6888063905605149584, -3.499999999999999556 ) ) ;
#4840 = CARTESIAN_POINT ( 'NONE',  ( 41.58830220609386430, 58.99948385550239749, 0.02388180880523263147 ) ) ;
#4841 = CARTESIAN_POINT ( 'NONE',  ( 52.29715082351547295, 64.39948385550239607, 6.992620115222774047 ) ) ;
#4842 = CARTESIAN_POINT ( 'NONE',  ( 4.124214193018072017, -4.056676826581893103, 6.968404583626299416E-17 ) ) ;
#4843 = MECHANICAL_DESIGN_GEOMETRIC_PRESENTATION_REPRESENTATION (  '', ( #8604 ), #10132 ) ;
#4844 = CARTESIAN_POINT ( 'NONE',  ( 47.42335538002188144, 50.59948385550240602, 8.007379884777233059 ) ) ;
#4845 = AXIS2_PLACEMENT_3D ( 'NONE', #7274, #11557, #13540 ) ;
#4846 = ORIENTED_EDGE ( 'NONE', *, *, #9911, .T. ) ;
#4847 = VERTEX_POINT ( 'NONE', #1818 ) ;
#4848 = EDGE_LOOP ( 'NONE', ( #2114, #8221, #11912, #10757, #309 ) ) ;
#4849 = ORIENTED_EDGE ( 'NONE', *, *, #8, .F. ) ;
#4850 = LINE ( 'NONE', #5894, #12774 ) ;
#4851 = LINE ( 'NONE', #8012, #10339 ) ;
#4852 = SHAPE_REPRESENTATION_RELATIONSHIP ( 'NONE' , 'NONE' ,  #11036, #12751 ) ;
#4853 = CARTESIAN_POINT ( 'NONE',  ( -5.999999999999921840, -32.99038105676662269, -9.000000000000000000 ) ) ;
#4854 = DIRECTION ( 'NONE',  ( -0.000000000000000000, -0.000000000000000000, 1.000000000000000000 ) ) ;
#4855 = PRODUCT_DEFINITION_FORMATION_WITH_SPECIFIED_SOURCE ( 'ANY', '', #13478, .NOT_KNOWN. ) ;
#4856 = DIRECTION ( 'NONE',  ( 0.000000000000000000, 1.000000000000000000, 0.000000000000000000 ) ) ;
#4857 = CIRCLE ( 'NONE', #8393, 1.499999999999999334 ) ;
#4858 = CARTESIAN_POINT ( 'NONE',  ( 48.02776887271745210, 61.39948385550240317, -5.992620115222778487 ) ) ;
#4859 = CARTESIAN_POINT ( 'NONE',  ( 56.65037692655921120, 55.10051614449766078, 2.184720259617097593 ) ) ;
#4860 = CARTESIAN_POINT ( 'NONE',  ( 52.57664461997821093, 57.40051614449767214, 8.007379884777206414 ) ) ;
#4861 = AXIS2_PLACEMENT_3D ( 'NONE', #13280, #3621, #615 ) ;
#4862 = DIRECTION ( 'NONE',  ( 0.000000000000000000, 0.000000000000000000, 1.000000000000000000 ) ) ;
#4863 = CARTESIAN_POINT ( 'NONE',  ( 50.76502259767569569, 44.99999999999998579, -6.467049654501940914 ) ) ;
#4864 = CARTESIAN_POINT ( 'NONE',  ( 57.36023556966787851, 61.00051614449766646, 0.02388180880515038476 ) ) ;
#4866 = ORIENTED_EDGE ( 'NONE', *, *, #7550, .T. ) ;
#4865 = EDGE_LOOP ( 'NONE', ( #8241, #5100, #4341, #11197 ) ) ;
#4867 = CIRCLE ( 'NONE', #2869, 12.50000000000000000 ) ;
#4868 = CARTESIAN_POINT ( 'NONE',  ( -1.654252653721913102, -3.663718938583024443, -0.01223254789874440342 ) ) ;
#4869 = ORIENTED_EDGE ( 'NONE', *, *, #9266, .T. ) ;
#4870 = EDGE_CURVE ( 'NONE', #13341, #5442, #5146, .T. ) ;
#4871 = DIRECTION ( 'NONE',  ( -0.000000000000000000, -0.000000000000000000, 1.000000000000000000 ) ) ;
#4872 = CARTESIAN_POINT ( 'NONE',  ( -1.000000000000000000, -14.00000000000000000, -9.000000000000001776 ) ) ;
#4873 = DIRECTION ( 'NONE',  ( -1.000000000000000000, 0.000000000000000000, 6.123233995736766036E-17 ) ) ;
#4874 = CARTESIAN_POINT ( 'NONE',  ( 53.54508667620428497, 46.29948385550240886, 4.840751629271157874 ) ) ;
#4875 = CARTESIAN_POINT ( 'NONE',  ( 55.94051828345050836, 59.79948385550240175, -4.345558710429103577 ) ) ;
#4876 =( BOUNDED_SURFACE ( )  B_SPLINE_SURFACE ( 3, 2, ( 
 ( #5870, #2881, #1763 ),
 ( #7103, #11312, #13167 ),
 ( #1834, #6083, #8909 ),
 ( #9036, #13104, #3648 ),
 ( #7870, #12079, #2598 ),
 ( #6826, #1551, #11032 ) ),
 .UNSPECIFIED., .F., .F., .T. ) 
 B_SPLINE_SURFACE_WITH_KNOTS ( ( 4, 2, 4 ),
 ( 3, 3 ),
 ( 0.02368235114939812314, 0.02663560780161266378, 0.02958886445382720443 ),
 ( 0.000000000000000000, 1.000000000000000000 ),
 .UNSPECIFIED. ) 
 GEOMETRIC_REPRESENTATION_ITEM ( )  RATIONAL_B_SPLINE_SURFACE ( (
 ( 1.000000000000000000, 0.8047780980783513227, 1.000000000000000000),
 ( 1.000000000000000000, 0.8123789398383446381, 1.000000000000000000),
 ( 1.000000000000000000, 0.8190677725692530053, 1.000000000000000000),
 ( 1.000000000000000000, 0.8192346316605858547, 1.000000000000000000),
 ( 1.000000000000000000, 0.8126126875065289301, 1.000000000000000000),
 ( 1.000000000000000000, 0.8047712635281869531, 1.000000000000000000) ) ) 
 REPRESENTATION_ITEM ( '' )  SURFACE ( )  );
#4877 = MECHANICAL_DESIGN_GEOMETRIC_PRESENTATION_REPRESENTATION (  '', ( #9 ), #229 ) ;
#4878 = VECTOR ( 'NONE', #4508, 1000.000000000000000 ) ;
#4879 = DIRECTION ( 'NONE',  ( 0.8660254037844450359, -0.4999999999999888423, 0.000000000000000000 ) ) ;
#4880 = DIRECTION ( 'NONE',  ( 0.000000000000000000, 0.000000000000000000, 1.000000000000000000 ) ) ;
#4881 = DIRECTION ( 'NONE',  ( 0.000000000000000000, 0.000000000000000000, 1.000000000000000000 ) ) ;
#4882 = CARTESIAN_POINT ( 'NONE',  ( 53.54508667620424234, 62.70051614449766220, -4.840751629271188961 ) ) ;
#4883 = CARTESIAN_POINT ( 'NONE',  ( 55.11794222512601493, 50.19948385550241454, 3.688883143319541702 ) ) ;
#4884 = CARTESIAN_POINT ( 'NONE',  ( 0.000000000000000000, 0.000000000000000000, 0.000000000000000000 ) ) ;
#4885 = ORIENTED_EDGE ( 'NONE', *, *, #11473, .T. ) ;
#4886 = ORIENTED_EDGE ( 'NONE', *, *, #7173, .F. ) ;
#4887 = VERTEX_POINT ( 'NONE', #2936 ) ;
#4888 = CARTESIAN_POINT ( 'NONE',  ( 45.60000000000000142, 0.000000000000000000, 2.055000000000000160 ) ) ;
#4889 = CARTESIAN_POINT ( 'NONE',  ( 6.204460410672267834, -4.828986228461502606, -1.635950503254466337 ) ) ;
#4890 = DIRECTION ( 'NONE',  ( -0.8660254037844355990, -0.5000000000000055511, 0.000000000000000000 ) ) ;
#4891 = DIRECTION ( 'NONE',  ( 0.000000000000000000, 0.000000000000000000, 1.000000000000000000 ) ) ;
#4892 = CARTESIAN_POINT ( 'NONE',  ( 55.94051828345053679, 61.20051614449766220, 4.345558710429044069 ) ) ;
#4893 = PLANE ( 'NONE',  #11264 ) ;
#4894 = CARTESIAN_POINT ( 'NONE',  ( 46.45491332379576477, 47.70051614449766220, 4.840751629271188961 ) ) ;
#4895 = CARTESIAN_POINT ( 'NONE',  ( 4.071447262713887127, 2.020725942163686284, -3.499999999999999556 ) ) ;
#4896 = CARTESIAN_POINT ( 'NONE',  ( 45.86712807150323812, 61.29948385550240886, -5.649768623646098220 ) ) ;
#4897 = CARTESIAN_POINT ( 'NONE',  ( 56.65037692655918988, 51.89948385550241028, -2.184720259617163762 ) ) ;
#4898 = CIRCLE ( 'NONE', #11526, 2.100000000000000089 ) ;
#4899 = EDGE_CURVE ( 'NONE', #6144, #11844, #8124, .T. ) ;
#4900 = CARTESIAN_POINT ( 'NONE',  ( 56.65037692655918988, 47.89948385550240317, -2.184720259617163762 ) ) ;
#4901 = EDGE_CURVE ( 'NONE', #967, #10505, #2863, .T. ) ;
#4902 = EDGE_LOOP ( 'NONE', ( #985, #4920, #3674 ) ) ;
#4903 = ORIENTED_EDGE ( 'NONE', *, *, #3130, .T. ) ;
#4904 = CYLINDRICAL_SURFACE ( 'NONE', #6816, 1.500000000000000444 ) ;
#4905 = EDGE_LOOP ( 'NONE', ( #3549, #8860, #12221, #12290 ) ) ;
#4906 = LINE ( 'NONE', #3718, #12469 ) ;
#4907 = AXIS2_PLACEMENT_3D ( 'NONE', #2649, #6871, #11079 ) ;
#4908 = CIRCLE ( 'NONE', #11966, 2.649999999999985700 ) ;
#4909 = CIRCLE ( 'NONE', #10420, 5.000000000000000888 ) ;
#4910 = DIRECTION ( 'NONE',  ( 1.000000000000000000, 0.000000000000000000, 0.000000000000000000 ) ) ;
#4911 = CARTESIAN_POINT ( 'NONE',  ( 55.08986747509849380, 59.20051614449766220, 3.727524721679155384 ) ) ;
#4912 = CARTESIAN_POINT ( 'NONE',  ( 4.000000000000000888, -0.8578082829538523635, -3.433262215449808696 ) ) ;
#4913 = CARTESIAN_POINT ( 'NONE',  ( 47.42335538002188144, 60.59948385550240602, 8.007379884777233059 ) ) ;
#4914 = B_SPLINE_CURVE_WITH_KNOTS ( 'NONE', 3,
 ( #12940, #6672, #10872, #599 ),
 .UNSPECIFIED., .F., .F.,
 ( 4, 4 ),
 ( 2.380735200829041677E-07, 0.002921158011986707288 ),
 .UNSPECIFIED. ) ;
#4915 = CARTESIAN_POINT ( 'NONE',  ( 55.94051828345050836, 63.79948385550240886, -4.345558710429104465 ) ) ;
#4916 = CARTESIAN_POINT ( 'NONE',  ( -4.197393957002303999, -0.8151795401431414234, -3.503767560748935139 ) ) ;
#4917 = CARTESIAN_POINT ( 'NONE',  ( 52.62207051974839089, 50.39948385550241738, 7.992620115222770494 ) ) ;
#4918 = AXIS2_PLACEMENT_3D ( 'NONE', #12543, #12670, #8268 ) ;
#4919 = EDGE_LOOP ( 'NONE', ( #12437, #7148 ) ) ;
#4920 = ORIENTED_EDGE ( 'NONE', *, *, #10510, .T. ) ;
#4921 = ORIENTED_EDGE ( 'NONE', *, *, #1952, .F. ) ;
#4922 = ORIENTED_EDGE ( 'NONE', *, *, #3228, .T. ) ;
#4923 = EDGE_CURVE ( 'NONE', #7907, #2486, #11154, .T. ) ;
#4924 = CARTESIAN_POINT ( 'NONE',  ( -2.449848172108560540, -3.432307619358754724, -3.503702292528910078 ) ) ;
#4925 = PLANE ( 'NONE',  #9241 ) ;
#4926 = CYLINDRICAL_SURFACE ( 'NONE', #7117, 4.799999999999999822 ) ;
#4927 = CARTESIAN_POINT ( 'NONE',  ( 0.000000000000000000, 0.000000000000000000, 3.469446951953614189E-15 ) ) ;
#4928 = LINE ( 'NONE', #8106, #8547 ) ;
#4929 = CARTESIAN_POINT ( 'NONE',  ( 49.97728705011488870, 65.49948385550240459, -6.000000000000000888 ) ) ;
#4930 = CARTESIAN_POINT ( 'NONE',  ( 43.34962307344078880, 54.10051614449766788, -2.184720259617096705 ) ) ;
#4931 = CARTESIAN_POINT ( 'NONE',  ( 42.39856655714564226, 60.10051614449766788, -2.493737253992044156 ) ) ;
#4932 = AXIS2_PLACEMENT_3D ( 'NONE', #9077, #1452, #3618 ) ;
#4933 = CARTESIAN_POINT ( 'NONE',  ( 1.171083334267915221, -24.65495046420793201, 9.000000000000000000 ) ) ;
#4934 = CARTESIAN_POINT ( 'NONE',  ( 4.000000000000000000, 2.309401076758515803, -0.4999999999999995559 ) ) ;
#4935 = EDGE_CURVE ( 'NONE', #4186, #12042, #4803, .T. ) ;
#4936 = CARTESIAN_POINT ( 'NONE',  ( 43.18075615816994173, 51.80051614449766362, 4.924951120819380357 ) ) ;
#4937 = ADVANCED_FACE ( 'NONE', ( #5089 ), #48, .T. ) ;
#4939 = ORIENTED_EDGE ( 'NONE', *, *, #5049, .F. ) ;
#4938 = ORIENTED_EDGE ( 'NONE', *, *, #12761, .T. ) ;
#4940 = CLOSED_SHELL ( 'NONE', ( #192, #5048, #1710, #6216, #1793, #5265 ) ) ;
#4941 = CARTESIAN_POINT ( 'NONE',  ( 0.6448876103708359731, 4.246476118072354922, -0.2256878752776725616 ) ) ;
#4942 = EDGE_LOOP ( 'NONE', ( #5457, #897, #2767, #12205 ) ) ;
#4943 = ORIENTED_EDGE ( 'NONE', *, *, #12589, .T. ) ;
#4944 = CARTESIAN_POINT ( 'NONE',  ( 0.4465819873852006072, 2.886751345948123770, -5.000000000000000000 ) ) ;
#4945 = LINE ( 'NONE', #1668, #7768 ) ;
#4946 = APPLICATION_PROTOCOL_DEFINITION ( 'draft international standard', 'automotive_design', 1998, #8051 ) ;
#4947 = CARTESIAN_POINT ( 'NONE',  ( 49.97728705011488870, 45.49948385550240459, -6.000000000000000888 ) ) ;
#4948 = CARTESIAN_POINT ( 'NONE',  ( 55.96859303347805081, 62.19948385550241454, 4.306917132069425058 ) ) ;
#4949 = CARTESIAN_POINT ( 'NONE',  ( 0.2174200650117537048, -2.185595227304857335, 3.214438021527933564 ) ) ;
#4950 = DIRECTION ( 'NONE',  ( 9.710251638871371392E-17, 5.969973981896233748E-17, 1.000000000000000000 ) ) ;
#4951 = CARTESIAN_POINT ( 'NONE',  ( -3.309651814758565180, -5.455921364805393026, -1.000000000000000000 ) ) ;
#4952 = ADVANCED_FACE ( 'NONE', ( #1673 ), #10191, .F. ) ;
#4953 = CARTESIAN_POINT ( 'NONE',  ( 43.34962307344078880, 52.10051614449766078, -2.184720259617096705 ) ) ;
#4954 = CARTESIAN_POINT ( 'NONE',  ( 49.97728705011488870, 53.49948385550240459, -6.000000000000000888 ) ) ;
#4955 = FACE_OUTER_BOUND ( 'NONE', #11712, .T. ) ;
#4956 = AXIS2_PLACEMENT_3D ( 'NONE', #3643, #5794, #6693 ) ;
#4957 = ORIENTED_EDGE ( 'NONE', *, *, #910, .F. ) ;
#4958 = EDGE_LOOP ( 'NONE', ( #3252, #8711, #12908, #9791 ) ) ;
#4959 = VERTEX_POINT ( 'NONE', #3004 ) ;
#4960 = CARTESIAN_POINT ( 'NONE',  ( 75.00000000000000000, 32.50000000000001421, -9.999999999999998224 ) ) ;
#4961 = B_SPLINE_CURVE_WITH_KNOTS ( 'NONE', 3,
 ( #1796, #6044, #11134, #5762, #12110, #8033 ),
 .UNSPECIFIED., .F., .F.,
 ( 4, 2, 4 ),
 ( 0.005339748439308726613, 0.006800846765732536554, 0.008261945092156346496 ),
 .UNSPECIFIED. ) ;
#4962 = DIRECTION ( 'NONE',  ( 9.710251638871371392E-17, 5.969973981896233748E-17, 1.000000000000000000 ) ) ;
#4963 = CARTESIAN_POINT ( 'NONE',  ( 6.207671477328757348, -5.338259717474211463, -0.7538629453363940858 ) ) ;
#4964 = CARTESIAN_POINT ( 'NONE',  ( 50.02271294988512551, 46.49948385550240459, 7.000000000000000888 ) ) ;
#4965 = VECTOR ( 'NONE', #11573, 1000.000000000000000 ) ;
#4966 = CARTESIAN_POINT ( 'NONE',  ( 1.925929944387235853E-31, 15.00000000000001599, 9.000000000000000000 ) ) ;
#4967 = CARTESIAN_POINT ( 'NONE',  ( 53.50833635130544508, 45.30051614449766362, 4.867452303228181343 ) ) ;
#4968 = DIRECTION ( 'NONE',  ( 1.000000000000000000, 0.000000000000000000, 0.000000000000000000 ) ) ;
#4969 = AXIS2_PLACEMENT_3D ( 'NONE', #1894, #12546, #8342 ) ;
#4970 = CARTESIAN_POINT ( 'NONE',  ( 56.66441430157296821, 58.09948385550240602, 2.141517661632100111 ) ) ;
#4971 = CARTESIAN_POINT ( 'NONE',  ( 50.02271294988512551, 50.49948385550240459, 7.000000000000000888 ) ) ;
#4972 = AXIS2_PLACEMENT_3D ( 'NONE', #10561, #5323, #9529 ) ;
#4973 = ORIENTED_EDGE ( 'NONE', *, *, #9143, .T. ) ;
#4974 = CARTESIAN_POINT ( 'NONE',  ( 55.94051828345050836, 51.79948385550240175, -4.345558710429104465 ) ) ;
#4975 = CIRCLE ( 'NONE', #6736, 2.149999999999999023 ) ;
#4976 = ORIENTED_EDGE ( 'NONE', *, *, #1649, .F. ) ;
#4977 = ORIENTED_EDGE ( 'NONE', *, *, #11744, .T. ) ;
#4978 = DIRECTION ( 'NONE',  ( -1.000000000000000000, 0.000000000000000000, 1.224646799147353207E-16 ) ) ;
#4979 = VERTEX_POINT ( 'NONE', #11435 ) ;
#4980 = CARTESIAN_POINT ( 'NONE',  ( 6.534838248920900483, -5.903531555104836848, 4.671345613696493211E-16 ) ) ;
#4981 = AXIS2_PLACEMENT_3D ( 'NONE', #12216, #8077, #4968 ) ;
#4982 = CYLINDRICAL_SURFACE ( 'NONE', #5847, 12.50000000000000000 ) ;
#4983 = PLANE ( 'NONE',  #856 ) ;
#4984 = CARTESIAN_POINT ( 'NONE',  ( 44.28664221472221385, 59.90051614449767214, 1.832500667257213722 ) ) ;
#4985 = CARTESIAN_POINT ( 'NONE',  ( 5.991014884144048480, 4.330127018922193649, 2.500000000000001776 ) ) ;
#4986 = CIRCLE ( 'NONE', #13102, 15.00000000000000000 ) ;
#4987 = CARTESIAN_POINT ( 'NONE',  ( 56.81924384183011512, 58.19948385550240744, 4.924951120819313743 ) ) ;
#4988 = CARTESIAN_POINT ( 'NONE',  ( 54.13287192849676188, 64.29948385550241596, 5.649768623646098220 ) ) ;
#4989 = FACE_OUTER_BOUND ( 'NONE', #4558, .T. ) ;
#4990 = CARTESIAN_POINT ( 'NONE',  ( 52.57664461997811856, 49.59948385550241312, -8.007379884777229506 ) ) ;
#4991 = EDGE_LOOP ( 'NONE', ( #10372, #3860, #3957, #13130 ) ) ;
#4992 = ORIENTED_EDGE ( 'NONE', *, *, #9519, .T. ) ;
#4993 = ORIENTED_EDGE ( 'NONE', *, *, #13346, .T. ) ;
#4994 = FACE_OUTER_BOUND ( 'NONE', #11553, .T. ) ;
#4995 = CARTESIAN_POINT ( 'NONE',  ( 25.00000000000000711, -20.00000000000000000, -23.00000000000000000 ) ) ;
#4996 = CARTESIAN_POINT ( 'NONE',  ( -5.999999999999921840, -32.99038105676662269, 9.000000000000000000 ) ) ;
#4997 = CARTESIAN_POINT ( 'NONE',  ( 4.078421086530217288, -3.990950201428958621, 0.000000000000000000 ) ) ;
#4998 = CARTESIAN_POINT ( 'NONE',  ( 0.1481481481481481122, -4.797713218419819903, -1.000000000000000000 ) ) ;
#4999 = CARTESIAN_POINT ( 'NONE',  ( 56.30877334542961421, 59.99948385550241170, -0.02388180880520959434 ) ) ;
#5000 = CARTESIAN_POINT ( 'NONE',  ( 44.03140696652198471, 53.80051614449766362, 4.306917132069485454 ) ) ;
#5001 = EDGE_CURVE ( 'NONE', #5304, #6641, #5801, .T. ) ;
#5002 = CARTESIAN_POINT ( 'NONE',  ( 50.02271294988505446, 58.50051614449765225, -8.000000000000001776 ) ) ;
#5003 = CARTESIAN_POINT ( 'NONE',  ( -7.499999999999998224, -20.00000000000000000, -20.00000000000000000 ) ) ;
#5004 = CARTESIAN_POINT ( 'NONE',  ( 42.38452918213190657, 47.90051614449765793, 2.450534656007115508 ) ) ;
#5005 = CONICAL_SURFACE ( 'NONE', #12712, 3.309499999999999886, 0.7853981633974407295 ) ;
#5007 = ORIENTED_EDGE ( 'NONE', *, *, #13177, .F. ) ;
#5006 = ORIENTED_EDGE ( 'NONE', *, *, #9483, .T. ) ;
#5008 = ORIENTED_EDGE ( 'NONE', *, *, #2290, .T. ) ;
#5009 = UNCERTAINTY_MEASURE_WITH_UNIT (LENGTH_MEASURE( 1.000000000000000082E-05 ), #9177, 'distance_accuracy_value', 'NONE');
#5010 = ORIENTED_EDGE ( 'NONE', *, *, #2126, .F. ) ;
#5011 = EDGE_CURVE ( 'NONE', #8586, #5283, #9412, .T. ) ;
#5012 = ORIENTED_EDGE ( 'NONE', *, *, #8650, .T. ) ;
#5013 = EDGE_CURVE ( 'NONE', #4232, #3196, #4689, .T. ) ;
#5014 = EDGE_CURVE ( 'NONE', #2384, #4657, #921, .T. ) ;
#5015 = CARTESIAN_POINT ( 'NONE',  ( -12.99038105676654453, -27.50000000000006040, 9.000000000000000000 ) ) ;
#5016 = DIRECTION ( 'NONE',  ( -1.000000000000000000, -0.000000000000000000, -0.000000000000000000 ) ) ;
#5017 = EDGE_CURVE ( 'NONE', #10229, #4573, #10114, .T. ) ;
#5018 = APPLICATION_PROTOCOL_DEFINITION ( 'draft international standard', 'automotive_design', 1998, #6128 ) ;
#5019 = CARTESIAN_POINT ( 'NONE',  ( 44.30067958973596376, 46.89948385550240317, 1.875703265242204099 ) ) ;
#5020 = CARTESIAN_POINT ( 'NONE',  ( 49.97728705011488159, 61.49948385550240459, -7.000000000000000888 ) ) ;
#5021 = AXIS2_PLACEMENT_3D ( 'NONE', #1654, #5898, #10095 ) ;
#5022 = DIRECTION ( 'NONE',  ( 0.000000000000000000, 0.000000000000000000, 1.000000000000000000 ) ) ;
#5023 = DIRECTION ( 'NONE',  ( -0.000000000000000000, -0.000000000000000000, -1.000000000000000000 ) ) ;
#5024 = PLANE ( 'NONE',  #2622 ) ;
#5025 = CARTESIAN_POINT ( 'NONE',  ( 45.86712807150329496, 53.70051614449766220, 5.649768623646139964 ) ) ;
#5026 = CARTESIAN_POINT ( 'NONE',  ( 44.88205777487398507, 55.19948385550240744, -3.688883143319540814 ) ) ;
#5027 = CYLINDRICAL_SURFACE ( 'NONE', #6513, 2.500000000000000444 ) ;
#5028 = VERTEX_POINT ( 'NONE', #6339 ) ;
#5029 = ORIENTED_EDGE ( 'NONE', *, *, #13527, .T. ) ;
#5030 = VERTEX_POINT ( 'NONE', #4376 ) ;
#5031 = FACE_OUTER_BOUND ( 'NONE', #10088, .T. ) ;
#5032 = CARTESIAN_POINT ( 'NONE',  ( 45.60000000000000142, 0.000000000000000000, 0.000000000000000000 ) ) ;
#5033 = CARTESIAN_POINT ( 'NONE',  ( 6.534838248920896930, -2.951765777552406878, 5.112608298763836601 ) ) ;
#5034 = ADVANCED_FACE ( 'NONE', ( #3210 ), #9432, .F. ) ;
#5035 =( LENGTH_UNIT ( ) NAMED_UNIT ( * ) SI_UNIT ( .MILLI., .METRE. ) );
#5036 = PRESENTATION_STYLE_ASSIGNMENT (( #6081 ) ) ;
#5037 = DIRECTION ( 'NONE',  ( -0.000000000000000000, -0.000000000000000000, -1.000000000000000000 ) ) ;
#5038 = CARTESIAN_POINT ( 'NONE',  ( 46.49166364869456913, 46.30051614449766362, -4.867452303228181343 ) ) ;
#5039 = DIRECTION ( 'NONE',  ( 1.000000000000000000, 0.000000000000000000, 0.000000000000000000 ) ) ;
#5040 = CARTESIAN_POINT ( 'NONE',  ( 57.36023556966787851, 57.99948385550239038, -0.02388180880522424582 ) ) ;
#5041 = CARTESIAN_POINT ( 'NONE',  ( 47.70284917648453415, 55.39948385550238896, -6.992620115222774047 ) ) ;
#5042 = ORIENTED_EDGE ( 'NONE', *, *, #4759, .T. ) ;
#5043 = CARTESIAN_POINT ( 'NONE',  ( 47.74827507625478518, 46.59948385550239891, 7.007379884777227730 ) ) ;
#5044 = ORIENTED_EDGE ( 'NONE', *, *, #6545, .T. ) ;
#5045 = DIRECTION ( 'NONE',  ( -0.000000000000000000, 0.000000000000000000, -1.000000000000000000 ) ) ;
#5046 = ORIENTED_EDGE ( 'NONE', *, *, #7493, .T. ) ;
#5047 = DIRECTION ( 'NONE',  ( 0.000000000000000000, -1.000000000000000000, 0.000000000000000000 ) ) ;
#5048 = ADVANCED_FACE ( 'NONE', ( #979 ), #912, .T. ) ;
#5049 = EDGE_CURVE ( 'NONE', #4365, #5652, #2640, .T. ) ;
#5050 = DIRECTION ( 'NONE',  ( -9.858538378746663627E-23, 5.031452844637890958E-23, -1.000000000000000000 ) ) ;
#5051 = CARTESIAN_POINT ( 'NONE',  ( 3.309651814758565180, -5.455921364805393026, -1.000000000000000000 ) ) ;
#5052 = CARTESIAN_POINT ( 'NONE',  ( 44.91013252490150620, 62.20051614449766220, -3.727524721679154940 ) ) ;
#5053 = VECTOR ( 'NONE', #3877, 1000.000000000000000 ) ;
#5054 = CARTESIAN_POINT ( 'NONE',  ( 4.197310751797292738, 0.8178363989516252985, -3.502498386812444409 ) ) ;
#5055 = CARTESIAN_POINT ( 'NONE',  ( 45.27934281921075410, 59.29948385550240886, -6.458785618021043895 ) ) ;
#5056 = LINE ( 'NONE', #13460, #7144 ) ;
#5057 = CARTESIAN_POINT ( 'NONE',  ( 42.38452918213188525, 51.09948385550240602, -2.450534656007040013 ) ) ;
#5058 = ORIENTED_EDGE ( 'NONE', *, *, #1456, .T. ) ;
#5059 = ORIENTED_EDGE ( 'NONE', *, *, #7552, .F. ) ;
#5060 = ORIENTED_EDGE ( 'NONE', *, *, #6966, .F. ) ;
#5061 = DIRECTION ( 'NONE',  ( 0.000000000000000000, 0.000000000000000000, 1.000000000000000000 ) ) ;
#5062 =( GEOMETRIC_REPRESENTATION_CONTEXT ( 3 ) GLOBAL_UNCERTAINTY_ASSIGNED_CONTEXT ( ( #506 ) ) GLOBAL_UNIT_ASSIGNED_CONTEXT ( ( #4482, #11107, #12150 ) ) REPRESENTATION_CONTEXT ( 'NONE', 'WORKASPACE' ) );
#5063 = FILL_AREA_STYLE_COLOUR ( '', #5104 ) ;
#5064 = DIRECTION ( 'NONE',  ( 0.000000000000000000, -0.000000000000000000, 1.000000000000000000 ) ) ;
#5065 = DIRECTION ( 'NONE',  ( -0.9768494444668812671, -0.2139279384389642935, 0.000000000000000000 ) ) ;
#5066 = CARTESIAN_POINT ( 'NONE',  ( -0.1410422978106123659, 4.700232962125094893, -3.687027686973624707 ) ) ;
#5067 = CARTESIAN_POINT ( 'NONE',  ( 44.88205777487398507, 65.19948385550240744, -3.688883143319540814 ) ) ;
#5068 = CARTESIAN_POINT ( 'NONE',  ( 50.02271294988505446, 50.50051614449765935, -7.000000000000000888 ) ) ;
#5069 = CARTESIAN_POINT ( 'NONE',  ( 49.97728705011495265, 61.50051614449766646, 8.000000000000001776 ) ) ;
#5070 = VECTOR ( 'NONE', #7443, 1000.000000000000000 ) ;
#5071 = CARTESIAN_POINT ( 'NONE',  ( 2.500000000000000444, 0.000000000000000000, -5.000000000000000888 ) ) ;
#5072 = ADVANCED_FACE ( 'NONE', ( #5364 ), #6466, .F. ) ;
#5073 = CARTESIAN_POINT ( 'NONE',  ( 41.58830220609386430, 50.00051614449765935, -0.02388180880514929535 ) ) ;
#5074 = AXIS2_PLACEMENT_3D ( 'NONE', #5713, #435, #10193 ) ;
#5075 = VECTOR ( 'NONE', #5634, 1000.000000000000000 ) ;
#5077 = ORIENTED_EDGE ( 'NONE', *, *, #7819, .F. ) ;
#5076 = ORIENTED_EDGE ( 'NONE', *, *, #9792, .F. ) ;
#5078 = ORIENTED_EDGE ( 'NONE', *, *, #1464, .T. ) ;
#5079 = VERTEX_POINT ( 'NONE', #6276 ) ;
#5080 = EDGE_CURVE ( 'NONE', #6586, #9257, #11873, .T. ) ;
#5081 = PRESENTATION_LAYER_ASSIGNMENT (  '', '', ( #4406 ) ) ;
#5082 = CARTESIAN_POINT ( 'NONE',  ( 6.495567275915080430, 5.834887664329775347, 9.410860448829699171E-16 ) ) ;
#5083 = VECTOR ( 'NONE', #730, 1000.000000000000000 ) ;
#5084 = DIRECTION ( 'NONE',  ( 0.000000000000000000, 0.000000000000000000, 1.000000000000000000 ) ) ;
#5085 = DIRECTION ( 'NONE',  ( 0.000000000000000000, 0.000000000000000000, 1.000000000000000000 ) ) ;
#5086 = SHAPE_DEFINITION_REPRESENTATION ( #10744, #10956 ) ;
#5087 = CARTESIAN_POINT ( 'NONE',  ( 54.13287192849676188, 64.29948385550241596, 5.649768623646098220 ) ) ;
#5088 = CARTESIAN_POINT ( 'NONE',  ( 52.29715082351547295, 60.39948385550240317, 6.992620115222774047 ) ) ;
#5089 = FACE_OUTER_BOUND ( 'NONE', #7593, .T. ) ;
#5090 = CARTESIAN_POINT ( 'NONE',  ( -14.92500000000000249, -18.50187617334218970, 0.000000000000000000 ) ) ;
#5091 = AXIS2_PLACEMENT_3D ( 'NONE', #9645, #1532, #3690 ) ;
#5092 = DIRECTION ( 'NONE',  ( -1.000000000000000000, 0.000000000000000000, 0.000000000000000000 ) ) ;
#5093 = CARTESIAN_POINT ( 'NONE',  ( 42.63976443033212860, 50.00051614449766646, -0.02388180880514948964 ) ) ;
#5094 = CARTESIAN_POINT ( 'NONE',  ( 51.97223112728254790, 52.39948385550241028, 5.992620115222778487 ) ) ;
#5095 = CIRCLE ( 'NONE', #2644, 1.999999999999998224 ) ;
#5096 = DIRECTION ( 'NONE',  ( 0.000000000000000000, 0.000000000000000000, -1.000000000000000000 ) ) ;
#5097 = ORIENTED_EDGE ( 'NONE', *, *, #11961, .T. ) ;
#5098 = CARTESIAN_POINT ( 'NONE',  ( 4.200000000000001954, 0.000000000000000000, 2.000000000000000888 ) ) ;
#5099 = ORIENTED_EDGE ( 'NONE', *, *, #4240, .F. ) ;
#5100 = ORIENTED_EDGE ( 'NONE', *, *, #11853, .F. ) ;
#5101 = CARTESIAN_POINT ( 'NONE',  ( 0.000000000000000000, 0.000000000000000000, -1.000000000000000000 ) ) ;
#5102 = CARTESIAN_POINT ( 'NONE',  ( 14.14213562373094923, -14.99999999999999112, -20.00000000000000000 ) ) ;
#5103 = CARTESIAN_POINT ( 'NONE',  ( 2.000000000000000000, -0.8865213383406730374, -1.535499999999999421 ) ) ;
#5104 = COLOUR_RGB ( '',0.8941176470588234615, 0.8941176470588234615, 0.8941176470588234615 ) ;
#5105 = CARTESIAN_POINT ( 'NONE',  ( 1.925929944387235853E-31, 15.00000000000001599, 9.000000000000000000 ) ) ;
#5106 = CIRCLE ( 'NONE', #2432, 5.000000000000000888 ) ;
#5107 = DIRECTION ( 'NONE',  ( 1.000000000000000000, 0.000000000000000000, 0.000000000000000000 ) ) ;
#5108 = CARTESIAN_POINT ( 'NONE',  ( 56.30877334542961421, 45.00051614449765225, 0.02388180880515774693 ) ) ;
#5109 = PLANE ( 'NONE',  #11137 ) ;
#5110 = CARTESIAN_POINT ( 'NONE',  ( 4.000000000000000000, -1.560351142792952617, -0.2242961665059816367 ) ) ;
#5111 = CARTESIAN_POINT ( 'NONE',  ( 54.13287192849676188, 56.29948385550240175, 5.649768623646098220 ) ) ;
#5112 = ORIENTED_EDGE ( 'NONE', *, *, #2212, .T. ) ;
#5113 = EDGE_CURVE ( 'NONE', #9080, #10006, #1181, .T. ) ;
#5114 = CARTESIAN_POINT ( 'NONE',  ( 52.29715082351547295, 48.39948385550240317, 6.992620115222774047 ) ) ;
#5115 = ADVANCED_FACE ( 'NONE', ( #10534 ), #5164, .F. ) ;
#5116 = AXIS2_PLACEMENT_3D ( 'NONE', #5139, #2986, #8443 ) ;
#5117 = VERTEX_POINT ( 'NONE', #13630 ) ;
#5118 = CARTESIAN_POINT ( 'NONE',  ( 3.972058292797711054, 0.6948821373584146421, 3.565770528409240026 ) ) ;
#5119 = ORIENTED_EDGE ( 'NONE', *, *, #11441, .F. ) ;
#5120 = EDGE_CURVE ( 'NONE', #10107, #6120, #4178, .T. ) ;
#5121 = CARTESIAN_POINT ( 'NONE',  ( 4.082498951862916670, 2.020725942163688504, 3.500000000000000000 ) ) ;
#5122 = LINE ( 'NONE', #12429, #742 ) ;
#5123 = CARTESIAN_POINT ( 'NONE',  ( 50.02271294988512551, 48.49948385550240459, 7.000000000000000888 ) ) ;
#5124 = AXIS2_PLACEMENT_3D ( 'NONE', #12829, #3172, #8560 ) ;
#5125 = CARTESIAN_POINT ( 'NONE',  ( 49.97728705011495265, 49.50051614449765935, 7.000000000000000888 ) ) ;
#5126 = CARTESIAN_POINT ( 'NONE',  ( -4.000000000000000000, 1.941961291383472732, -0.3515519931180205448 ) ) ;
#5127 = CARTESIAN_POINT ( 'NONE',  ( 43.18075615816989199, 57.19948385550241454, -4.924951120819313743 ) ) ;
#5128 = DIRECTION ( 'NONE',  ( -1.000000000000000000, 1.734723475976807094E-16, 0.000000000000000000 ) ) ;
#5129 = CARTESIAN_POINT ( 'NONE',  ( 58.41169779390614281, 49.99948385550240459, -0.02388180880523160798 ) ) ;
#5130 = VERTEX_POINT ( 'NONE', #12800 ) ;
#5131 = CIRCLE ( 'NONE', #679, 3.500000000000000000 ) ;
#5132 = ORIENTED_EDGE ( 'NONE', *, *, #3382, .F. ) ;
#5133 = ORIENTED_EDGE ( 'NONE', *, *, #10454, .F. ) ;
#5134 = VECTOR ( 'NONE', #8954, 1000.000000000000000 ) ;
#5135 = B_SPLINE_CURVE_WITH_KNOTS ( 'NONE', 3,
 ( #7583, #7854, #8619, #1259, #12065, #9853 ),
 .UNSPECIFIED., .F., .F.,
 ( 4, 2, 4 ),
 ( 0.002365888236227995517, 0.003551327329835084114, 0.004736766423442172712 ),
 .UNSPECIFIED. ) ;
#5136 = DIRECTION ( 'NONE',  ( 1.000000000000000000, 0.000000000000000000, 0.000000000000000000 ) ) ;
#5137 = B_SPLINE_CURVE_WITH_KNOTS ( 'NONE', 3,
 ( #6423, #12418, #3160, #5313, #11388, #12625 ),
 .UNSPECIFIED., .F., .F.,
 ( 4, 2, 4 ),
 ( 0.01308430720669670130, 0.01410661709916351952, 0.01512892699163033601 ),
 .UNSPECIFIED. ) ;
#5138 = CARTESIAN_POINT ( 'NONE',  ( -7.499999999999923617, -32.99038105676662269, -9.000000000000000000 ) ) ;
#5139 = CARTESIAN_POINT ( 'NONE',  ( 0.000000000000000000, 0.000000000000000000, 0.000000000000000000 ) ) ;
#5140 = EDGE_CURVE ( 'NONE', #3165, #5335, #12539, .T. ) ;
#5141 = CARTESIAN_POINT ( 'NONE',  ( 3.453038570460273071, 2.625189405340834448, -3.535263753543585352 ) ) ;
#5142 = CARTESIAN_POINT ( 'NONE',  ( 46.49166364869460466, 60.69948385550240033, 4.867452303228209765 ) ) ;
#5143 = CARTESIAN_POINT ( 'NONE',  ( 50.02271294988505446, 62.50051614449766646, -7.000000000000000888 ) ) ;
#5144 = CARTESIAN_POINT ( 'NONE',  ( 42.38452918213190657, 59.90051614449767214, 2.450534656007115508 ) ) ;
#5145 = AXIS2_PLACEMENT_3D ( 'NONE', #8466, #9500, #3213 ) ;
#5146 = CIRCLE ( 'NONE', #1802, 0.4999999999999978351 ) ;
#5147 = CARTESIAN_POINT ( 'NONE',  ( 4.000000000000000000, 0.7924765000094659007, -0.05906175389889852662 ) ) ;
#5148 = CARTESIAN_POINT ( 'NONE',  ( 47.42335538002180328, 52.40051614449767214, -8.007379884777206414 ) ) ;
#5150 = ORIENTED_EDGE ( 'NONE', *, *, #427, .T. ) ;
#5149 = VERTEX_POINT ( 'NONE', #3342 ) ;
#5151 = EDGE_CURVE ( 'NONE', #8098, #10200, #9497, .T. ) ;
#5152 = VERTEX_POINT ( 'NONE', #2158 ) ;
#5153 = UNCERTAINTY_MEASURE_WITH_UNIT (LENGTH_MEASURE( 1.000000000000000082E-05 ), #4129, 'distance_accuracy_value', 'NONE');
#5154 = EDGE_LOOP ( 'NONE', ( #13463, #2133 ) ) ;
#5155 = LINE ( 'NONE', #9690, #1441 ) ;
#5156 = CARTESIAN_POINT ( 'NONE',  ( 0.000000000000000000, 5.773502691896261751, -2.749426538070115714E-16 ) ) ;
#5157 = CARTESIAN_POINT ( 'NONE',  ( 1.925929944387235853E-31, 15.00000000000001599, 9.000000000000000000 ) ) ;
#5158 = CARTESIAN_POINT ( 'NONE',  ( -2.649999999999987477, 15.00000000000001599, 15.00000000000000178 ) ) ;
#5159 = ITEM_DEFINED_TRANSFORMATION ( 'NONE', 'NONE', #1294,  #430 ) ;
#5160 = CARTESIAN_POINT ( 'NONE',  ( 45.90387839640214196, 64.69948385550240744, 5.676469297603166098 ) ) ;
#5161 = CARTESIAN_POINT ( 'NONE',  ( 54.13287192849676188, 58.29948385550240175, 5.649768623646098220 ) ) ;
#5162 = CARTESIAN_POINT ( 'NONE',  ( 45.86712807150329496, 61.70051614449766220, 5.649768623646139964 ) ) ;
#5163 = AXIS2_PLACEMENT_3D ( 'NONE', #2215, #4367, #5549 ) ;
#5164 = CYLINDRICAL_SURFACE ( 'NONE', #4026, 2.149999999999999023 ) ;
#5165 = LINE ( 'NONE', #7160, #5456 ) ;
#5166 = CARTESIAN_POINT ( 'NONE',  ( 49.99999999999997158, 45.00000000000001421, -7.499999999999998224 ) ) ;
#5167 = CARTESIAN_POINT ( 'NONE',  ( 43.33558569842706021, 49.90051614449766504, 2.141517661632167169 ) ) ;
#5168 = CARTESIAN_POINT ( 'NONE',  ( 55.69932041026404335, 49.89948385550241028, -1.875703265242203432 ) ) ;
#5169 = DIRECTION ( 'NONE',  ( 0.000000000000000000, 0.000000000000000000, -1.000000000000000000 ) ) ;
#5170 = ORIENTED_EDGE ( 'NONE', *, *, #12034, .T. ) ;
#5171 = CARTESIAN_POINT ( 'NONE',  ( -1.498123826657872470, -5.075000000000001066, -9.000000000000000000 ) ) ;
#5172 = ORIENTED_EDGE ( 'NONE', *, *, #11926, .F. ) ;
#5173 = VERTEX_POINT ( 'NONE', #8534 ) ;
#5174 = CARTESIAN_POINT ( 'NONE',  ( 0.5000000000000000000, -6.429618962271402616, -1.000000000000000000 ) ) ;
#5175 = CARTESIAN_POINT ( 'NONE',  ( 6.362374563308228481, 5.433808049139812191, -0.8060918076009558897 ) ) ;
#5176 = CARTESIAN_POINT ( 'NONE',  ( 6.207530437345013752, -3.810448612250145750, -3.400109403952246367 ) ) ;
#5177 = CARTESIAN_POINT ( 'NONE',  ( 54.13287192849676188, 46.29948385550240886, 5.649768623646098220 ) ) ;
#5178 = CARTESIAN_POINT ( 'NONE',  ( -2.807080416178626692, 3.225969019225154444, -3.502507215260441065 ) ) ;
#5179 = CARTESIAN_POINT ( 'NONE',  ( 46.49166364869456913, 48.30051614449765651, -4.867452303228181343 ) ) ;
#5180 = DIRECTION ( 'NONE',  ( 0.000000000000000000, -0.5000000000000011102, -0.8660254037844379305 ) ) ;
#5181 = DIRECTION ( 'NONE',  ( 1.000000000000000000, -0.000000000000000000, 0.000000000000000000 ) ) ;
#5182 = CARTESIAN_POINT ( 'NONE',  ( 44.05948171654949874, 50.79948385550238754, 4.345558710429105354 ) ) ;
#5183 = ORIENTED_EDGE ( 'NONE', *, *, #6781, .T. ) ;
#5184 = CARTESIAN_POINT ( 'NONE',  ( 52.25172492374522903, 53.59948385550241312, -7.007379884777225953 ) ) ;
#5185 = VERTEX_POINT ( 'NONE', #10603 ) ;
#5186 = CARTESIAN_POINT ( 'NONE',  ( 4.158806752148102248, -2.089318365061878513, 3.500000000000000000 ) ) ;
#5187 = ORIENTED_EDGE ( 'NONE', *, *, #9129, .T. ) ;
#5188 = EDGE_CURVE ( 'NONE', #331, #9574, #4246, .T. ) ;
#5189 = AXIS2_PLACEMENT_3D ( 'NONE', #2578, #6803, #11008 ) ;
#5190 = DIRECTION ( 'NONE',  ( -0.000000000000000000, -0.000000000000000000, -1.000000000000000000 ) ) ;
#5191 = FACE_OUTER_BOUND ( 'NONE', #841, .T. ) ;
#5192 = EDGE_CURVE ( 'NONE', #2677, #12170, #11702, .T. ) ;
#5193 = DIRECTION ( 'NONE',  ( 1.000000000000000000, 0.000000000000000000, 0.000000000000000000 ) ) ;
#5194 = AXIS2_PLACEMENT_3D ( 'NONE', #10470, #10333, #5096 ) ;
#5195 = EDGE_CURVE ( 'NONE', #10003, #9042, #4908, .T. ) ;
#5196 = CARTESIAN_POINT ( 'NONE',  ( 49.97728705011495265, 47.50051614449766646, 7.000000000000000888 ) ) ;
#5197 = EDGE_CURVE ( 'NONE', #6904, #6584, #10399, .T. ) ;
#5198 = CYLINDRICAL_SURFACE ( 'NONE', #13662, 1.500000000000001332 ) ;
#5199 = AXIS2_PLACEMENT_3D ( 'NONE', #6113, #7209, #8316 ) ;
#5200 = CARTESIAN_POINT ( 'NONE',  ( 43.20883090819745576, 62.79948385550240175, 4.963592699179006473 ) ) ;
#5201 = FACE_OUTER_BOUND ( 'NONE', #6375, .T. ) ;
#5202 = AXIS2_PLACEMENT_3D ( 'NONE', #11396, #5190, #1918 ) ;
#5203 = EDGE_CURVE ( 'NONE', #9576, #5420, #7345, .T. ) ;
#5204 = CARTESIAN_POINT ( 'NONE',  ( 57.61547081786812896, 54.09948385550241312, 2.450534656007040901 ) ) ;
#5205 = ORIENTED_EDGE ( 'NONE', *, *, #1266, .F. ) ;
#5206 = AXIS2_PLACEMENT_3D ( 'NONE', #4198, #6152, #932 ) ;
#5207 = VERTEX_POINT ( 'NONE', #415 ) ;
#5208 = PLANE ( 'NONE',  #2403 ) ;
#5209 = CIRCLE ( 'NONE', #12905, 0.2000000000000000944 ) ;
#5210 = DIRECTION ( 'NONE',  ( -1.000000000000000000, 9.251858538542972814E-17, -0.000000000000000000 ) ) ;
#5211 = EDGE_CURVE ( 'NONE', #2490, #10214, #1122, .T. ) ;
#5212 = CARTESIAN_POINT ( 'NONE',  ( 6.541171661047877173, -5.920857802016179505, -0.02973393389965061501 ) ) ;
#5213 = DIRECTION ( 'NONE',  ( 1.000000000000000000, 0.000000000000000000, -0.000000000000000000 ) ) ;
#5214 = CARTESIAN_POINT ( 'NONE',  ( 55.71335778527780036, 46.90051614449766504, -1.832500667257213056 ) ) ;
#5215 = ADVANCED_FACE ( 'NONE', ( #10733 ), #7634, .T. ) ;
#5216 = CARTESIAN_POINT ( 'NONE',  ( 54.13287192849671214, 62.70051614449766220, -5.649768623646139964 ) ) ;
#5217 = CARTESIAN_POINT ( 'NONE',  ( 57.60143344285433642, 45.89948385550240317, -2.493737253992118319 ) ) ;
#5218 = DIRECTION ( 'NONE',  ( 0.000000000000000000, 0.000000000000000000, 1.000000000000000000 ) ) ;
#5219 = CARTESIAN_POINT ( 'NONE',  ( 45.31609314410960820, 48.30051614449765651, -6.485486291978072693 ) ) ;
#5220 = VERTEX_POINT ( 'NONE', #8873 ) ;
#5221 = ORIENTED_EDGE ( 'NONE', *, *, #6349, .F. ) ;
#5222 = EDGE_LOOP ( 'NONE', ( #12478, #8571, #8386, #7811 ) ) ;
#5223 = CARTESIAN_POINT ( 'NONE',  ( 6.436591462021357124, 5.789018756751930894, -2.883547477572278442E-16 ) ) ;
#5224 = CARTESIAN_POINT ( 'NONE',  ( 6.436591462021363341, 2.894509378375959674, -5.013437306331780086 ) ) ;
#5225 = CARTESIAN_POINT ( 'NONE',  ( -22.14999999999999858, -19.99999999999999289, -20.00000000000000000 ) ) ;
#5226 = CARTESIAN_POINT ( 'NONE',  ( 4.071447262713887127, -2.020725942163686284, 3.500000000000000444 ) ) ;
#5227 = CARTESIAN_POINT ( 'NONE',  ( 49.97728705011488870, 49.49948385550241170, -6.000000000000000888 ) ) ;
#5228 = EDGE_CURVE ( 'NONE', #6586, #6035, #8671, .T. ) ;
#5229 = DIRECTION ( 'NONE',  ( 0.000000000000000000, 1.000000000000000000, -1.224646799147353207E-16 ) ) ;
#5230 = CARTESIAN_POINT ( 'NONE',  ( 57.36023556966787851, 59.00051614449765935, 0.02388180880515038476 ) ) ;
#5231 = CARTESIAN_POINT ( 'NONE',  ( 6.244297270354683960, 1.802013835206515036E-11, 5.105276777067893512 ) ) ;
#5232 = CARTESIAN_POINT ( 'NONE',  ( -14.99999999999999645, -20.00000000000005329, -9.000000000000000000 ) ) ;
#5233 = LINE ( 'NONE', #1044, #5357 ) ;
#5234 = CARTESIAN_POINT ( 'NONE',  ( 54.09612160359792199, 49.30051614449765651, 5.676469297603124353 ) ) ;
#5235 = CARTESIAN_POINT ( 'NONE',  ( 44.28664221472220675, 57.09948385550240602, -1.832500667257165317 ) ) ;
#5236 = CARTESIAN_POINT ( 'NONE',  ( 20.00000000000000000, -20.00000000000000000, -12.00000000000000000 ) ) ;
#5237 = ORIENTED_EDGE ( 'NONE', *, *, #10900, .T. ) ;
#5238 = DIRECTION ( 'NONE',  ( 0.000000000000000000, 0.5000000000000018874, 0.8660254037844375974 ) ) ;
#5239 = ORIENTED_EDGE ( 'NONE', *, *, #12441, .T. ) ;
#5240 = ORIENTED_EDGE ( 'NONE', *, *, #9129, .F. ) ;
#5241 = CARTESIAN_POINT ( 'NONE',  ( 6.466260427357663154, 2.904280683598005730, 5.030361703432624232 ) ) ;
#5242 = VECTOR ( 'NONE', #1043, 1000.000000000000000 ) ;
#5243 = LINE ( 'NONE', #4260, #1175 ) ;
#5244 = CARTESIAN_POINT ( 'NONE',  ( 6.327640840229819652, -2.033197012992983943, 4.999999999998298250 ) ) ;
#5245 = VECTOR ( 'NONE', #3743, 1000.000000000000000 ) ;
#5246 = CARTESIAN_POINT ( 'NONE',  ( 10.00000000000000000, 15.00000000000001776, 15.00000000000000000 ) ) ;
#5247 = CARTESIAN_POINT ( 'NONE',  ( 44.28664221472221385, 53.90051614449765793, 1.832500667257213722 ) ) ;
#5248 = CARTESIAN_POINT ( 'NONE',  ( 6.196878017913831194, -5.292377467571572680, 0.8333333333333327042 ) ) ;
#5249 = CARTESIAN_POINT ( 'NONE',  ( 56.65037692655918988, 61.89948385550241028, -2.184720259617163762 ) ) ;
#5250 = CARTESIAN_POINT ( 'NONE',  ( 42.63976443033212860, 62.99948385550241170, 0.02388180880522514787 ) ) ;
#5251 = CARTESIAN_POINT ( 'NONE',  ( 56.65037692655918988, 61.89948385550241028, -2.184720259617163762 ) ) ;
#5252 = EDGE_CURVE ( 'NONE', #5998, #7289, #3477, .T. ) ;
#5253 = VERTEX_POINT ( 'NONE', #11837 ) ;
#5254 = ORIENTED_EDGE ( 'NONE', *, *, #11259, .T. ) ;
#5255 = CARTESIAN_POINT ( 'NONE',  ( -0.6810597143197697489, -4.461075778259609770, -3.598441714920717516 ) ) ;
#5256 = ADVANCED_FACE ( 'NONE', ( #1451 ), #1381, .F. ) ;
#5257 = CARTESIAN_POINT ( 'NONE',  ( 20.00000000000000000, -20.00000000000000000, -20.00000000000000000 ) ) ;
#5258 = PLANE ( 'NONE',  #6665 ) ;
#5259 = B_SPLINE_CURVE_WITH_KNOTS ( 'NONE', 3,
 ( #1399, #4536, #9789, #6493, #4395, #9724, #4466, #3433 ),
 .UNSPECIFIED., .F., .F.,
 ( 4, 2, 2, 4 ),
 ( 0.002921158011986710323, 0.003648658599403064445, 0.004376159186819419435, 0.005831160361652128546 ),
 .UNSPECIFIED. ) ;
#5260 = CARTESIAN_POINT ( 'NONE',  ( 4.175813232069150338, -4.122719923832746325, 2.362127131240695889E-16 ) ) ;
#5261 = CARTESIAN_POINT ( 'NONE',  ( 55.94051828345050836, 47.79948385550240886, -4.345558710429103577 ) ) ;
#5262 = CARTESIAN_POINT ( 'NONE',  ( 43.33558569842706021, 47.90051614449765793, 2.141517661632167169 ) ) ;
#5263 = DIRECTION ( 'NONE',  ( 0.000000000000000000, 0.000000000000000000, -1.000000000000000000 ) ) ;
#5264 = CARTESIAN_POINT ( 'NONE',  ( 47.70284917648453415, 47.39948385550238896, -6.992620115222774047 ) ) ;
#5265 = ADVANCED_FACE ( 'NONE', ( #12866 ), #3410, .F. ) ;
#5266 = CARTESIAN_POINT ( 'NONE',  ( 54.68390685589033495, 55.69948385550240744, -6.485486291978119766 ) ) ;
#5267 = ADVANCED_FACE ( 'NONE', ( #7839 ), #1312, .T. ) ;
#5268 = EDGE_LOOP ( 'NONE', ( #5405, #12646, #419, #2366 ) ) ;
#5269 = ADVANCED_FACE ( 'NONE', ( #4724 ), #9837, .F. ) ;
#5270 = ORIENTED_EDGE ( 'NONE', *, *, #13275, .F. ) ;
#5271 = CARTESIAN_POINT ( 'NONE',  ( 0.000000000000000000, 0.5192545390863916310, 0.000000000000000000 ) ) ;
#5272 = CARTESIAN_POINT ( 'NONE',  ( 75.00000000000002842, -39.99999999999998579, 10.00000000000000000 ) ) ;
#5273 = CARTESIAN_POINT ( 'NONE',  ( 6.207530437345012864, -4.849805425595699937, 1.599890596045217439 ) ) ;
#5274 = LINE ( 'NONE', #12516, #13602 ) ;
#5275 = CARTESIAN_POINT ( 'NONE',  ( 46.49166364869456913, 50.30051614449766362, -4.867452303228181343 ) ) ;
#5276 = CARTESIAN_POINT ( 'NONE',  ( 49.97728705011495265, 59.50051614449765935, 7.000000000000000888 ) ) ;
#5277 = CARTESIAN_POINT ( 'NONE',  ( 50.02271294988505446, 64.50051614449766646, -8.000000000000001776 ) ) ;
#5278 = CARTESIAN_POINT ( 'NONE',  ( 4.030867648404937498, 3.732851566701761659, 0.5345114293584584120 ) ) ;
#5279 = CARTESIAN_POINT ( 'NONE',  ( 56.79116909180259398, 59.20051614449766220, 4.963592699178938972 ) ) ;
#5280 = VECTOR ( 'NONE', #8206, 1000.000000000000000 ) ;
#5281 = ORIENTED_EDGE ( 'NONE', *, *, #1272, .T. ) ;
#5282 = CIRCLE ( 'NONE', #9686, 6.080745460913608902 ) ;
#5283 = VERTEX_POINT ( 'NONE', #356 ) ;
#5284 = EDGE_CURVE ( 'NONE', #8238, #2658, #9701, .T. ) ;
#5285 = ORIENTED_EDGE ( 'NONE', *, *, #8645, .F. ) ;
#5286 = CARTESIAN_POINT ( 'NONE',  ( 6.534533895392296010, 5.902695350657467088, 5.075181882648644095E-15 ) ) ;
#5287 = DIRECTION ( 'NONE',  ( 0.000000000000000000, 0.000000000000000000, 1.000000000000000000 ) ) ;
#5288 = CARTESIAN_POINT ( 'NONE',  ( 4.630153689607048761, 0.000000000000000000, 0.000000000000000000 ) ) ;
#5289 = CARTESIAN_POINT ( 'NONE',  ( 3.951447005078451813, 1.347150628109126558, 3.500000000000000444 ) ) ;
#5290 = CARTESIAN_POINT ( 'NONE',  ( 44.91013252490152752, 52.79948385550240175, 3.727524721679198461 ) ) ;
#5291 = VECTOR ( 'NONE', #6253, 1000.000000000000000 ) ;
#5292 = CARTESIAN_POINT ( 'NONE',  ( 45.86712807150323812, 63.29948385550240886, -5.649768623646098220 ) ) ;
#5293 = CARTESIAN_POINT ( 'NONE',  ( 45.31609314410960820, 48.30051614449765651, -6.485486291978072693 ) ) ;
#5294 = CIRCLE ( 'NONE', #3297, 1.500000000000001110 ) ;
#5295 = DIRECTION ( 'NONE',  ( -0.000000000000000000, -0.000000000000000000, -1.000000000000000000 ) ) ;
#5296 = CARTESIAN_POINT ( 'NONE',  ( -62.49999999999997158, 32.50000000000001421, -9.999999999999998224 ) ) ;
#5297 = CARTESIAN_POINT ( 'NONE',  ( 14.92499999999998650, -18.50187617334198009, 9.000000000000000000 ) ) ;
#5298 = CARTESIAN_POINT ( 'NONE',  ( 44.03140696652198471, 55.80051614449766362, 4.306917132069485454 ) ) ;
#5299 = CARTESIAN_POINT ( 'NONE',  ( 49.97728705011488870, 61.49948385550241170, -6.000000000000000888 ) ) ;
#5300 = CARTESIAN_POINT ( 'NONE',  ( 2.449293598294706513E-15, -20.00000000000000000, 9.999999999999998224 ) ) ;
#5301 = ORIENTED_EDGE ( 'NONE', *, *, #12335, .T. ) ;
#5302 =( GEOMETRIC_REPRESENTATION_CONTEXT ( 3 ) GLOBAL_UNCERTAINTY_ASSIGNED_CONTEXT ( ( #11728 ) ) GLOBAL_UNIT_ASSIGNED_CONTEXT ( ( #5726, #2594, #5929 ) ) REPRESENTATION_CONTEXT ( 'NONE', 'WORKASPACE' ) );
#5303 = DIRECTION ( 'NONE',  ( 0.000000000000000000, -0.8660254037844382635, -0.5000000000000008882 ) ) ;
#5304 = VERTEX_POINT ( 'NONE', #4585 ) ;
#5305 = CARTESIAN_POINT ( 'NONE',  ( 75.00000000000002842, -39.99999999999998579, 10.00000000000000000 ) ) ;
#5306 = CARTESIAN_POINT ( 'NONE',  ( -12.99038105676654453, -27.50000000000006040, -9.000000000000000000 ) ) ;
#5307 = CARTESIAN_POINT ( 'NONE',  ( 1.219878473194462964, -24.84890673354692936, 15.00000000000000355 ) ) ;
#5308 = CARTESIAN_POINT ( 'NONE',  ( 47.70284917648453415, 51.39948385550238896, -6.992620115222774047 ) ) ;
#5309 = AXIS2_PLACEMENT_3D ( 'NONE', #4664, #7849, #7712 ) ;
#5310 = AXIS2_PLACEMENT_3D ( 'NONE', #12605, #10532, #1040 ) ;
#5311 = CARTESIAN_POINT ( 'NONE',  ( -1.243802165048909503, 3.900692638707381921, -3.223146290109805800 ) ) ;
#5312 = CARTESIAN_POINT ( 'NONE',  ( 50.02271294988506156, 52.50051614449766646, -6.000000000000000888 ) ) ;
#5313 = CARTESIAN_POINT ( 'NONE',  ( 0.1381419387168661417, -1.355287006802423644, -3.499999999999999556 ) ) ;
#5314 = CARTESIAN_POINT ( 'NONE',  ( -29.99999999999999645, 0.000000000000000000, -10.00000000000000000 ) ) ;
#5315 = CARTESIAN_POINT ( 'NONE',  ( 54.13287192849676188, 62.29948385550240886, 5.649768623646098220 ) ) ;
#5316 = CARTESIAN_POINT ( 'NONE',  ( 44.05948171654949874, 62.79948385550241596, 4.345558710429105354 ) ) ;
#5317 = ORIENTED_EDGE ( 'NONE', *, *, #9234, .F. ) ;
#5318 = ORIENTED_EDGE ( 'NONE', *, *, #4567, .F. ) ;
#5319 = CARTESIAN_POINT ( 'NONE',  ( -1.390230914382372118, -4.043987460488664532, -3.502507215260523665 ) ) ;
#5320 = VECTOR ( 'NONE', #4756, 1000.000000000000000 ) ;
#5321 = FACE_OUTER_BOUND ( 'NONE', #1879, .T. ) ;
#5322 = CARTESIAN_POINT ( 'NONE',  ( 4.052424581287827010, -2.393186648133491357, 2.990837702970496892 ) ) ;
#5323 = DIRECTION ( 'NONE',  ( 0.000000000000000000, 0.000000000000000000, -1.000000000000000000 ) ) ;
#5324 = CARTESIAN_POINT ( 'NONE',  ( 54.09612160359786515, 47.69948385550240744, -5.676469297603166098 ) ) ;
#5325 = CARTESIAN_POINT ( 'NONE',  ( 48.07319477248762496, 64.40051614449764372, -6.007379884777208190 ) ) ;
#5326 = EDGE_CURVE ( 'NONE', #7674, #7202, #7109, .T. ) ;
#5327 = LINE ( 'NONE', #9336, #9716 ) ;
#5328 = SHAPE_REPRESENTATION ( 'MAS-183', ( #5091, #8390, #1294, #6204, #5519, #7510, #1077, #626, #9278, #5529, #5309, #13216, #13005, #8615, #214, #12141 ), #5969 ) ;
#5329 = CARTESIAN_POINT ( 'NONE',  ( 57.36023556966787851, 47.99948385550239038, -0.02388180880522424582 ) ) ;
#5330 = CARTESIAN_POINT ( 'NONE',  ( -29.99999999999999645, -40.00000000000000000, 10.00000000000000000 ) ) ;
#5331 = CIRCLE ( 'NONE', #13029, 4.800000000000000711 ) ;
#5332 = B_SPLINE_CURVE_WITH_KNOTS ( 'NONE', 3,
 ( #8984, #7949, #13456, #4839, #2687, #6913 ),
 .UNSPECIFIED., .F., .F.,
 ( 4, 2, 4 ),
 ( 0.01103795672827925789, 0.01206113196748797960, 0.01308430720669670130 ),
 .UNSPECIFIED. ) ;
#5333 = CARTESIAN_POINT ( 'NONE',  ( 52.57664461997811856, 59.59948385550240602, -8.007379884777229506 ) ) ;
#5334 = EDGE_LOOP ( 'NONE', ( #3997, #9660 ) ) ;
#5335 = VERTEX_POINT ( 'NONE', #6595 ) ;
#5336 = DIRECTION ( 'NONE',  ( 1.000000000000000000, 3.469446951953615175E-16, 0.000000000000000000 ) ) ;
#5337 = VECTOR ( 'NONE', #12075, 999.9999999999998863 ) ;
#5338 = DIRECTION ( 'NONE',  ( -0.000000000000000000, -0.000000000000000000, -1.000000000000000000 ) ) ;
#5339 = DIRECTION ( 'NONE',  ( -1.000000000000000000, 0.000000000000000000, 0.000000000000000000 ) ) ;
#5340 = CARTESIAN_POINT ( 'NONE',  ( 0.000000000000000000, 1.773042676681340524, -2.059984127722458425E-15 ) ) ;
#5341 = CARTESIAN_POINT ( 'NONE',  ( 49.97728705011494554, 45.50051614449766646, 6.000000000000000888 ) ) ;
#5342 = CARTESIAN_POINT ( 'NONE',  ( 54.09612160359792199, 57.30051614449765651, 5.676469297603124353 ) ) ;
#5343 = CARTESIAN_POINT ( 'NONE',  ( 45.31609314410967926, 46.69948385550240744, 6.485486291978119766 ) ) ;
#5344 = DIRECTION ( 'NONE',  ( -1.000000000000000000, 0.000000000000000000, 0.000000000000000000 ) ) ;
#5345 = CARTESIAN_POINT ( 'NONE',  ( 56.81924384183006538, 58.80051614449766362, -4.924951120819380357 ) ) ;
#5346 = CIRCLE ( 'NONE', #7991, 3.299999999999999822 ) ;
#5347 = VECTOR ( 'NONE', #7565, 1000.000000000000000 ) ;
#5349 = ADVANCED_FACE ( 'NONE', ( #12050 ), #5766, .F. ) ;
#5348 = VERTEX_POINT ( 'NONE', #13001 ) ;
#5350 = EDGE_LOOP ( 'NONE', ( #2275, #8805, #7287, #4434, #7792 ) ) ;
#5351 = ORIENTED_EDGE ( 'NONE', *, *, #12174, .T. ) ;
#5352 = FACE_OUTER_BOUND ( 'NONE', #552, .T. ) ;
#5353 = CARTESIAN_POINT ( 'NONE',  ( 0.000000000000000000, -4.330127018922188320, 2.500000000000010214 ) ) ;
#5354 = CARTESIAN_POINT ( 'NONE',  ( 50.00000000000000000, 15.00000000000000000, 0.000000000000000000 ) ) ;
#5355 = CARTESIAN_POINT ( 'NONE',  ( -4.211140560182196957, -2.431303136016552013, -3.745885042887436178 ) ) ;
#5356 = CARTESIAN_POINT ( 'NONE',  ( 2.649999999999987477, 15.00000000000001599, 15.00000000000000178 ) ) ;
#5357 = VECTOR ( 'NONE', #10467, 1000.000000000000000 ) ;
#5358 = CARTESIAN_POINT ( 'NONE',  ( 50.02271294988511841, 48.49948385550241170, 6.000000000000000888 ) ) ;
#5359 = CIRCLE ( 'NONE', #8882, 15.00000000000000000 ) ;
#5360 = CARTESIAN_POINT ( 'NONE',  ( 57.36023556966787851, 63.99948385550241170, -0.02388180880522424582 ) ) ;
#5361 = ADVANCED_FACE ( 'NONE', ( #10935 ), #13140, .T. ) ;
#5362 = CARTESIAN_POINT ( 'NONE',  ( 47.42335538002180328, 48.40051614449766504, -8.007379884777206414 ) ) ;
#5363 = ADVANCED_FACE ( 'NONE', ( #11773 ), #4653, .F. ) ;
#5364 = FACE_OUTER_BOUND ( 'NONE', #116, .T. ) ;
#5365 = CARTESIAN_POINT ( 'NONE',  ( 6.367873360227556567, 2.886751345948123770, -5.000000000000000000 ) ) ;
#5366 = CARTESIAN_POINT ( 'NONE',  ( 45.86712807150329496, 55.70051614449766220, 5.649768623646139964 ) ) ;
#5367 = CARTESIAN_POINT ( 'NONE',  ( 53.50833635130540955, 61.69948385550240744, -4.867452303228209765 ) ) ;
#5368 = LINE ( 'NONE', #93, #7181 ) ;
#5369 = ORIENTED_EDGE ( 'NONE', *, *, #2861, .T. ) ;
#5370 = CIRCLE ( 'NONE', #4697, 2.500000000000000444 ) ;
#5371 = FACE_OUTER_BOUND ( 'NONE', #3573, .T. ) ;
#5372 = ORIENTED_EDGE ( 'NONE', *, *, #81, .F. ) ;
#5373 = CARTESIAN_POINT ( 'NONE',  ( 6.495567275915077765, 2.917443832164883233, 5.053160945538031079 ) ) ;
#5374 = AXIS2_PLACEMENT_3D ( 'NONE', #7436, #10734, #4377 ) ;
#5375 = DIRECTION ( 'NONE',  ( 0.000000000000000000, -0.000000000000000000, 1.000000000000000000 ) ) ;
#5376 = CARTESIAN_POINT ( 'NONE',  ( 0.000000000000000000, 0.000000000000000000, -1.000000000000000000 ) ) ;
#5377 = CARTESIAN_POINT ( 'NONE',  ( 52.25172492374522903, 49.59948385550240602, -7.007379884777225953 ) ) ;
#5378 = ADVANCED_FACE ( 'NONE', ( #10997 ), #1016, .T. ) ;
#5379 = DIRECTION ( 'NONE',  ( -0.9768494444668813781, -0.2139279384389642935, 1.428280402115105433E-22 ) ) ;
#5380 = CARTESIAN_POINT ( 'NONE',  ( 44.30067958973594955, 50.10051614449766078, -1.875703265242155693 ) ) ;
#5381 = CARTESIAN_POINT ( 'NONE',  ( 4.175075985190095373, -2.060370777630118777, 3.568666869285566090 ) ) ;
#5382 = LINE ( 'NONE', #11600, #11884 ) ;
#5383 = DIRECTION ( 'NONE',  ( -1.000000000000000000, 0.000000000000000000, 0.000000000000000000 ) ) ;
#5384 = CARTESIAN_POINT ( 'NONE',  ( 44.05948171654949874, 56.79948385550240886, 4.345558710429105354 ) ) ;
#5385 = VECTOR ( 'NONE', #6616, 1000.000000000000000 ) ;
#5386 = CYLINDRICAL_SURFACE ( 'NONE', #1596, 2.100000000000000089 ) ;
#5387 = ORIENTED_EDGE ( 'NONE', *, *, #5284, .T. ) ;
#5388 = ORIENTED_EDGE ( 'NONE', *, *, #3011, .F. ) ;
#5389 = EDGE_CURVE ( 'NONE', #12172, #12511, #4079, .T. ) ;
#5390 = VERTEX_POINT ( 'NONE', #1997 ) ;
#5391 = CLOSED_SHELL ( 'NONE', ( #2239, #2401, #9796, #7868, #2600, #6860, #10966, #8008, #7639, #1097, #5267, #10324, #1095, #11114, #19, #10060, #297, #8036, #9928, #5532, #4679, #12368, #10672, #7299, #9542, #5439, #10422, #8088, #7691, #8897, #12890, #6773, #120, #2736, #3794, #5269, #2605 ) ) ;
#5392 = DIRECTION ( 'NONE',  ( -1.000000000000000000, 0.000000000000000000, 0.000000000000000000 ) ) ;
#5393 = AXIS2_PLACEMENT_3D ( 'NONE', #9562, #85, #787 ) ;
#5394 = DIRECTION ( 'NONE',  ( 0.000000000000000000, 0.000000000000000000, -1.000000000000000000 ) ) ;
#5395 = CARTESIAN_POINT ( 'NONE',  ( 3.973110223768737015, -0.6864646529411583264, -3.565797985667475078 ) ) ;
#5396 = DIRECTION ( 'NONE',  ( 0.000000000000000000, 0.000000000000000000, 1.000000000000000000 ) ) ;
#5397 = CARTESIAN_POINT ( 'NONE',  ( 57.36023556966787851, 53.99948385550239749, -0.02388180880522424582 ) ) ;
#5398 = CARTESIAN_POINT ( 'NONE',  ( 57.36023556966787851, 47.00051614449764514, 0.02388180880515038476 ) ) ;
#5399 = CARTESIAN_POINT ( 'NONE',  ( 75.00000000000001421, 2.602085213965211904E-14, 0.000000000000000000 ) ) ;
#5400 = CARTESIAN_POINT ( 'NONE',  ( 52.29715082351547295, 48.39948385550240317, 6.992620115222774047 ) ) ;
#5401 = DIRECTION ( 'NONE',  ( 0.000000000000000000, 0.000000000000000000, 1.000000000000000000 ) ) ;
#5402 = CARTESIAN_POINT ( 'NONE',  ( 50.02271294988513972, 54.49948385550240459, 8.000000000000001776 ) ) ;
#5403 = B_SPLINE_CURVE_WITH_KNOTS ( 'NONE', 3,
 ( #2941, #839, #6281, #9437, #2162, #9233 ),
 .UNSPECIFIED., .F., .F.,
 ( 4, 2, 4 ),
 ( 0.0007315534878134838555, 0.001060812114463466869, 0.001390070741113449884 ),
 .UNSPECIFIED. ) ;
#5404 = AXIS2_PLACEMENT_3D ( 'NONE', #5306, #6415, #4323 ) ;
#5405 = ORIENTED_EDGE ( 'NONE', *, *, #1158, .F. ) ;
#5406 = EDGE_LOOP ( 'NONE', ( #457, #11971, #12458, #101 ) ) ;
#5407 = CARTESIAN_POINT ( 'NONE',  ( 5.599999999999999645, 2.020725942163686284, -3.499999999999999556 ) ) ;
#5408 = CARTESIAN_POINT ( 'NONE',  ( 6.204460410672268722, -3.831267809382561840, 3.364049496746113199 ) ) ;
#5409 = LINE ( 'NONE', #2202, #4517 ) ;
#5410 = CARTESIAN_POINT ( 'NONE',  ( 56.30877334542961421, 49.00051614449765935, 0.02388180880515774693 ) ) ;
#5411 = CARTESIAN_POINT ( 'NONE',  ( 44.03140696652198471, 61.80051614449766362, 4.306917132069485454 ) ) ;
#5412 = AXIS2_PLACEMENT_3D ( 'NONE', #10944, #7709, #2438 ) ;
#5413 = CARTESIAN_POINT ( 'NONE',  ( 54.68390685589039890, 63.30051614449767072, 6.485486291978072693 ) ) ;
#5414 = FACE_OUTER_BOUND ( 'NONE', #6739, .T. ) ;
#5415 = AXIS2_PLACEMENT_3D ( 'NONE', #6410, #12673, #8201 ) ;
#5416 = CARTESIAN_POINT ( 'NONE',  ( 52.62207051974829852, 58.60051614449766788, -7.992620115222797139 ) ) ;
#5417 =( REPRESENTATION_RELATIONSHIP ('NONE','NONE', #5328, #7264 ) REPRESENTATION_RELATIONSHIP_WITH_TRANSFORMATION ( #1504 )SHAPE_REPRESENTATION_RELATIONSHIP( ) );
#5418 = AXIS2_PLACEMENT_3D ( 'NONE', #4209, #2967, #13660 ) ;
#5419 = ORIENTED_EDGE ( 'NONE', *, *, #6395, .F. ) ;
#5420 = VERTEX_POINT ( 'NONE', #13533 ) ;
#5421 = ORIENTED_EDGE ( 'NONE', *, *, #729, .T. ) ;
#5422 = AXIS2_PLACEMENT_3D ( 'NONE', #4071, #11465, #13658 ) ;
#5423 = DIRECTION ( 'NONE',  ( 0.000000000000000000, -0.000000000000000000, 1.000000000000000000 ) ) ;
#5424 =( NAMED_UNIT ( * ) PLANE_ANGLE_UNIT ( ) SI_UNIT ( $, .RADIAN. ) );
#5425 = EDGE_CURVE ( 'NONE', #9171, #12678, #9098, .T. ) ;
#5426 = CARTESIAN_POINT ( 'NONE',  ( -29.99999999999999645, 40.00000000000000000, 0.000000000000000000 ) ) ;
#5427 = B_SPLINE_CURVE_WITH_KNOTS ( 'NONE', 3,
 ( #5226, #9428, #7365, #5289, #7692 ),
 .UNSPECIFIED., .F., .F.,
 ( 4, 1, 4 ),
 ( 0.000000000000000000, 0.002020725942163687470, 0.004041451884327374941 ),
 .UNSPECIFIED. ) ;
#5428 = FACE_BOUND ( 'NONE', #1247, .T. ) ;
#5429 = MANIFOLD_SOLID_BREP ( 'M5 Clearance Hole1', #4940 ) ;
#5430 = CARTESIAN_POINT ( 'NONE',  ( 55.08986747509847248, 51.79948385550240175, -3.727524721679197572 ) ) ;
#5431 = DIRECTION ( 'NONE',  ( -0.000000000000000000, 0.000000000000000000, -1.000000000000000000 ) ) ;
#5432 = CARTESIAN_POINT ( 'NONE',  ( 43.20883090819742023, 46.20051614449766220, -4.963592699178938972 ) ) ;
#5433 = DIRECTION ( 'NONE',  ( -1.000000000000000000, 0.000000000000000000, 0.000000000000000000 ) ) ;
#5434 = CARTESIAN_POINT ( 'NONE',  ( 0.000000000000000000, 0.000000000000000000, -5.000000000000000888 ) ) ;
#5435 = CARTESIAN_POINT ( 'NONE',  ( 43.33558569842706021, 59.90051614449766504, 2.141517661632167169 ) ) ;
#5436 = CARTESIAN_POINT ( 'NONE',  ( 51.92680522751233951, 61.59948385550240602, -6.007379884777223289 ) ) ;
#5437 = EDGE_CURVE ( 'NONE', #12919, #3041, #2781, .T. ) ;
#5438 = ORIENTED_EDGE ( 'NONE', *, *, #8889, .F. ) ;
#5439 = ADVANCED_FACE ( 'NONE', ( #5976 ), #7904, .F. ) ;
#5440 = CARTESIAN_POINT ( 'NONE',  ( 1.411581201560190495E-15, 4.862606272033091592, -3.745885042887436622 ) ) ;
#5441 = EDGE_CURVE ( 'NONE', #5875, #568, #10639, .T. ) ;
#5442 = VERTEX_POINT ( 'NONE', #8369 ) ;
#5443 = CARTESIAN_POINT ( 'NONE',  ( 52.80949999999998568, 0.000000000000000000, 4.000000000000000000 ) ) ;
#5444 = EDGE_CURVE ( 'NONE', #10373, #9556, #4674, .T. ) ;
#5445 = CARTESIAN_POINT ( 'NONE',  ( -2.500000000000000888, 0.000000000000000000, -4.974599999999998801 ) ) ;
#5446 = CARTESIAN_POINT ( 'NONE',  ( 2.000000000000008882, 3.464101615137749945, 0.000000000000000000 ) ) ;
#5447 = CARTESIAN_POINT ( 'NONE',  ( 44.03140696652192787, 53.19948385550238612, -4.306917132069425058 ) ) ;
#5448 = DIRECTION ( 'NONE',  ( 1.000000000000000000, 0.000000000000000000, 0.000000000000000000 ) ) ;
#5449 = CARTESIAN_POINT ( 'NONE',  ( 55.08986747509849380, 51.20051614449766220, 3.727524721679155384 ) ) ;
#5450 = DIRECTION ( 'NONE',  ( -0.000000000000000000, -0.000000000000000000, 1.000000000000000000 ) ) ;
#5451 = CARTESIAN_POINT ( 'NONE',  ( 6.244889965166094292, 3.924082311521017274, 3.413878157001050795 ) ) ;
#5452 = PRESENTATION_STYLE_ASSIGNMENT (( #1205 ) ) ;
#5453 = CARTESIAN_POINT ( 'NONE',  ( 49.97728705011488159, 59.49948385550240459, -7.000000000000000888 ) ) ;
#5454 = DIRECTION ( 'NONE',  ( 0.000000000000000000, 0.000000000000000000, -1.000000000000000000 ) ) ;
#5455 = ORIENTED_EDGE ( 'NONE', *, *, #10264, .T. ) ;
#5456 = VECTOR ( 'NONE', #12540, 1000.000000000000000 ) ;
#5457 = ORIENTED_EDGE ( 'NONE', *, *, #10999, .F. ) ;
#5458 = ORIENTED_EDGE ( 'NONE', *, *, #6601, .T. ) ;
#5459 = FACE_BOUND ( 'NONE', #9985, .T. ) ;
#5460 = CARTESIAN_POINT ( 'NONE',  ( 0.1999999999999987899, 4.041334437186265510E-16, -3.299999999999999822 ) ) ;
#5461 = CARTESIAN_POINT ( 'NONE',  ( 3.958484000407985981, -2.327740518749076948, 2.968235154689861321 ) ) ;
#5462 = CARTESIAN_POINT ( 'NONE',  ( -2.000000000000000000, -6.429618962271402616, 0.000000000000000000 ) ) ;
#5463 = CARTESIAN_POINT ( 'NONE',  ( 54.13287192849676188, 54.29948385550240886, 5.649768623646098220 ) ) ;
#5464 = CARTESIAN_POINT ( 'NONE',  ( 47.74827507625469281, 52.40051614449763662, -7.007379884777203749 ) ) ;
#5465 = CARTESIAN_POINT ( 'NONE',  ( -62.49999999999997158, 32.50000000000001421, 15.00000000000000000 ) ) ;
#5466 = CARTESIAN_POINT ( 'NONE',  ( 42.39856655714566358, 62.89948385550240317, 2.493737253992119207 ) ) ;
#5467 = SURFACE_SIDE_STYLE ('',( #2194 ) ) ;
#5468 = CARTESIAN_POINT ( 'NONE',  ( 58.41169779390614281, 55.99948385550241170, -0.02388180880523160798 ) ) ;
#5469 = ORIENTED_EDGE ( 'NONE', *, *, #6407, .T. ) ;
#5470 = EDGE_CURVE ( 'NONE', #8026, #5335, #6148, .T. ) ;
#5471 = ORIENTED_EDGE ( 'NONE', *, *, #1348, .F. ) ;
#5472 = DIRECTION ( 'NONE',  ( 0.000000000000000000, 0.000000000000000000, 1.000000000000000000 ) ) ;
#5473 = CARTESIAN_POINT ( 'NONE',  ( -30.00000000000000000, -40.00000000000000000, 12.50000000000000000 ) ) ;
#5474 = CARTESIAN_POINT ( 'NONE',  ( 55.69932041026405045, 45.10051614449766788, 1.875703265242156359 ) ) ;
#5475 = CARTESIAN_POINT ( 'NONE',  ( 1.267864665251833278E-11, -20.00000000000000000, 9.000000000000000000 ) ) ;
#5476 = CARTESIAN_POINT ( 'NONE',  ( 45.31609314410967926, 48.69948385550241454, 6.485486291978119766 ) ) ;
#5477 = DIRECTION ( 'NONE',  ( -0.000000000000000000, 0.000000000000000000, -1.000000000000000000 ) ) ;
#5478 = CARTESIAN_POINT ( 'NONE',  ( 57.61547081786810764, 56.90051614449767214, -2.450534656007114176 ) ) ;
#5479 = EDGE_LOOP ( 'NONE', ( #6283, #4031, #1647 ) ) ;
#5480 = VERTEX_POINT ( 'NONE', #13271 ) ;
#5481 = ORIENTED_EDGE ( 'NONE', *, *, #11322, .T. ) ;
#5482 = MECHANICAL_DESIGN_GEOMETRIC_PRESENTATION_REPRESENTATION (  '', ( #2828 ), #2373 ) ;
#5483 = ORIENTED_EDGE ( 'NONE', *, *, #12589, .F. ) ;
#5484 = CARTESIAN_POINT ( 'NONE',  ( 3.734041964264196434, -16.98388816369253362, -8.999999999999996447 ) ) ;
#5485 = SURFACE_SIDE_STYLE ('',( #9762 ) ) ;
#5486 = DIRECTION ( 'NONE',  ( -0.000000000000000000, -0.000000000000000000, 1.000000000000000000 ) ) ;
#5487 = PRESENTATION_STYLE_ASSIGNMENT (( #1239 ) ) ;
#5488 = CARTESIAN_POINT ( 'NONE',  ( 53.54508667620428497, 52.29948385550240886, 4.840751629271157874 ) ) ;
#5489 = CARTESIAN_POINT ( 'NONE',  ( -59.84999999999998721, 32.50000000000001421, 9.999999999999998224 ) ) ;
#5490 = CARTESIAN_POINT ( 'NONE',  ( 52.62207051974829852, 44.60051614449766078, -7.992620115222797139 ) ) ;
#5491 =( REPRESENTATION_RELATIONSHIP ('NONE','NONE', #5328, #5848 ) REPRESENTATION_RELATIONSHIP_WITH_TRANSFORMATION ( #5889 )SHAPE_REPRESENTATION_RELATIONSHIP( ) );
#5492 = AXIS2_PLACEMENT_3D ( 'NONE', #4275, #4403, #8493 ) ;
#5493 = DIRECTION ( 'NONE',  ( -0.000000000000000000, -0.000000000000000000, 1.000000000000000000 ) ) ;
#5494 = LINE ( 'NONE', #4445, #6037 ) ;
#5495 = CARTESIAN_POINT ( 'NONE',  ( 49.97728705011495265, 59.50051614449765935, 7.000000000000000888 ) ) ;
#5496 = CARTESIAN_POINT ( 'NONE',  ( 51.97223112728254790, 56.39948385550241028, 5.992620115222778487 ) ) ;
#5497 = EDGE_CURVE ( 'NONE', #11125, #7907, #3135, .T. ) ;
#5498 = ORIENTED_EDGE ( 'NONE', *, *, #11044, .T. ) ;
#5499 = CARTESIAN_POINT ( 'NONE',  ( 1.567478505476134606E-15, 4.618802153517012066, -3.433295621305382905 ) ) ;
#5500 = ORIENTED_EDGE ( 'NONE', *, *, #9083, .F. ) ;
#5501 = CARTESIAN_POINT ( 'NONE',  ( 2.000000000000000000, 2.065682573263594481E-15, 1.535500000000000309 ) ) ;
#5502 = CIRCLE ( 'NONE', #3065, 2.396904916527700102 ) ;
#5503 = CARTESIAN_POINT ( 'NONE',  ( 5.100000000000002309, 0.000000000000000000, 0.000000000000000000 ) ) ;
#5504 = DIRECTION ( 'NONE',  ( 0.000000000000000000, 0.000000000000000000, 1.000000000000000000 ) ) ;
#5505 = PRESENTATION_LAYER_ASSIGNMENT (  '', '', ( #10353 ) ) ;
#5506 =( LENGTH_UNIT ( ) NAMED_UNIT ( * ) SI_UNIT ( .MILLI., .METRE. ) );
#5507 = CARTESIAN_POINT ( 'NONE',  ( 54.13287192849676188, 48.29948385550240175, 5.649768623646098220 ) ) ;
#5508 = CARTESIAN_POINT ( 'NONE',  ( 4.211140560182196957, -2.431303136016555122, -3.745885042887436622 ) ) ;
#5509 = CARTESIAN_POINT ( 'NONE',  ( 48.07319477248762496, 50.40051614449766504, -6.007379884777208190 ) ) ;
#5510 = FACE_OUTER_BOUND ( 'NONE', #10923, .T. ) ;
#5511 = CARTESIAN_POINT ( 'NONE',  ( -65.14999999999996305, 32.50000000000001421, -9.999999999999998224 ) ) ;
#5512 = CARTESIAN_POINT ( 'NONE',  ( 47.70284917648453415, 61.39948385550241738, -6.992620115222774047 ) ) ;
#5513 = DIRECTION ( 'NONE',  ( 1.000000000000000000, 0.000000000000000000, 0.000000000000000000 ) ) ;
#5514 = ORIENTED_EDGE ( 'NONE', *, *, #2577, .T. ) ;
#5515 = AXIS2_PLACEMENT_3D ( 'NONE', #12806, #1457, #7503 ) ;
#5516 = ORIENTED_EDGE ( 'NONE', *, *, #7972, .F. ) ;
#5517 = CARTESIAN_POINT ( 'NONE',  ( 0.1756481739660539498, -4.720212674038995360, -3.469390959564070620 ) ) ;
#5518 = CARTESIAN_POINT ( 'NONE',  ( -8.759913291900476295, -7.823632761846195827, 0.000000000000000000 ) ) ;
#5519 = AXIS2_PLACEMENT_3D ( 'NONE', #13014, #3758, #1462 ) ;
#5520 = PLANE ( 'NONE',  #2897 ) ;
#5521 = CARTESIAN_POINT ( 'NONE',  ( -12.17636723815377309, -28.75991329190052070, 9.000000000000000000 ) ) ;
#5522 = CARTESIAN_POINT ( 'NONE',  ( 43.33558569842703179, 51.09948385550240602, -2.141517661632099223 ) ) ;
#5523 = CARTESIAN_POINT ( 'NONE',  ( 47.70284917648459100, 51.60051614449765367, 6.992620115222796251 ) ) ;
#5524 = CARTESIAN_POINT ( 'NONE',  ( 0.000000000000000000, 0.000000000000000000, -5.000000000000000000 ) ) ;
#5525 = CARTESIAN_POINT ( 'NONE',  ( 50.02271294988512551, 54.49948385550240459, 7.000000000000000888 ) ) ;
#5526 = EDGE_CURVE ( 'NONE', #13574, #10214, #11476, .T. ) ;
#5527 = FILL_AREA_STYLE ('',( #6507 ) ) ;
#5528 = ADVANCED_FACE ( 'NONE', ( #5201 ), #2707, .T. ) ;
#5529 = AXIS2_PLACEMENT_3D ( 'NONE', #9847, #6873, #7913 ) ;
#5530 = CARTESIAN_POINT ( 'NONE',  ( 41.58830220609386430, 64.99948385550240459, 0.02388180880523263147 ) ) ;
#5531 = CIRCLE ( 'NONE', #1988, 5.000000000000000888 ) ;
#5532 = ADVANCED_FACE ( 'NONE', ( #11139 ), #193, .T. ) ;
#5533 = ORIENTED_EDGE ( 'NONE', *, *, #7633, .T. ) ;
#5534 = ORIENTED_EDGE ( 'NONE', *, *, #9649, .T. ) ;
#5535 = CARTESIAN_POINT ( 'NONE',  ( 2.100000000000000089, 0.000000000000000000, -0.2800830152838844622 ) ) ;
#5536 = CARTESIAN_POINT ( 'NONE',  ( -13.67449106481164733, -26.16508670809959725, 0.000000000000000000 ) ) ;
#5537 = CARTESIAN_POINT ( 'NONE',  ( 44.88205777487401349, 51.80051614449766362, 3.688883143319584779 ) ) ;
#5538 = CIRCLE ( 'NONE', #12596, 2.499999999999999556 ) ;
#5539 = DIRECTION ( 'NONE',  ( -1.000000000000000000, 0.000000000000000000, 0.000000000000000000 ) ) ;
#5540 = CARTESIAN_POINT ( 'NONE',  ( 56.81924384183011512, 50.19948385550241454, 4.924951120819313743 ) ) ;
#5541 = CARTESIAN_POINT ( 'NONE',  ( 55.94051828345050836, 53.79948385550238754, -4.345558710429104465 ) ) ;
#5542 = CARTESIAN_POINT ( 'NONE',  ( 75.00000000000001421, -39.99999999999998579, -10.00000000000000000 ) ) ;
#5543 = CARTESIAN_POINT ( 'NONE',  ( 42.38452918213190657, 57.90051614449765793, 2.450534656007115508 ) ) ;
#5544 = VERTEX_POINT ( 'NONE', #12903 ) ;
#5545 = VERTEX_POINT ( 'NONE', #8635 ) ;
#5546 = ORIENTED_EDGE ( 'NONE', *, *, #11849, .T. ) ;
#5547 = ORIENTED_EDGE ( 'NONE', *, *, #5704, .F. ) ;
#5548 = AXIS2_PLACEMENT_3D ( 'NONE', #12981, #8923, #10978 ) ;
#5549 = DIRECTION ( 'NONE',  ( 1.000000000000000000, 0.000000000000000000, 0.000000000000000000 ) ) ;
#5550 =( NAMED_UNIT ( * ) SI_UNIT ( $, .STERADIAN. ) SOLID_ANGLE_UNIT ( ) );
#5551 =( NAMED_UNIT ( * ) SI_UNIT ( $, .STERADIAN. ) SOLID_ANGLE_UNIT ( ) );
#5552 = CARTESIAN_POINT ( 'NONE',  ( 0.1996310553826632361, 1.947030205581113282, 4.999999999999997335 ) ) ;
#5553 = DIRECTION ( 'NONE',  ( 0.000000000000000000, 0.000000000000000000, 1.000000000000000000 ) ) ;
#5554 = CARTESIAN_POINT ( 'NONE',  ( 48.02776887271745210, 59.39948385550240317, -5.992620115222778487 ) ) ;
#5555 = CARTESIAN_POINT ( 'NONE',  ( 57.36023556966787851, 45.00051614449765225, 0.02388180880515038476 ) ) ;
#5556 = CARTESIAN_POINT ( 'NONE',  ( 47.37792948025170858, 49.60051614449766788, 7.992620115222797139 ) ) ;
#5557 = AXIS2_PLACEMENT_3D ( 'NONE', #3705, #13031, #5866 ) ;
#5558 = DIRECTION ( 'NONE',  ( 1.000000000000000000, -1.734723475976807341E-16, 0.000000000000000000 ) ) ;
#5559 = CARTESIAN_POINT ( 'NONE',  ( 3.260336594487419859, -23.79080536174652494, -9.999999999999994671 ) ) ;
#5560 = EDGE_CURVE ( 'NONE', #13026, #9340, #8440, .T. ) ;
#5561 = CARTESIAN_POINT ( 'NONE',  ( 54.13287192849671214, 54.70051614449766220, -5.649768623646139964 ) ) ;
#5562 = CARTESIAN_POINT ( 'NONE',  ( 46.49166364869460466, 62.69948385550240744, 4.867452303228209765 ) ) ;
#5563 = ORIENTED_EDGE ( 'NONE', *, *, #11474, .F. ) ;
#5564 = CARTESIAN_POINT ( 'NONE',  ( 1.498123826657866253, -34.92499999999999716, 0.000000000000000000 ) ) ;
#5565 = VERTEX_POINT ( 'NONE', #6568 ) ;
#5566 = CARTESIAN_POINT ( 'NONE',  ( 0.000000000000000000, 0.5192545390863916310, 0.000000000000000000 ) ) ;
#5567 = CIRCLE ( 'NONE', #6020, 0.4999999999999972244 ) ;
#5568 = PRODUCT_DEFINITION_SHAPE ( 'NONE', 'NONE',  #13668 ) ;
#5569 = VECTOR ( 'NONE', #6732, 1000.000000000000000 ) ;
#5570 = DIRECTION ( 'NONE',  ( -9.710251638871371392E-17, -5.969973981896233748E-17, -1.000000000000000000 ) ) ;
#5571 = CARTESIAN_POINT ( 'NONE',  ( 3.972066048304772501, -3.435565134476469495, -1.180968096049828775 ) ) ;
#5572 = CARTESIAN_POINT ( 'NONE',  ( 56.66441430157296821, 52.09948385550240602, 2.141517661632100111 ) ) ;
#5573 = PRODUCT_RELATED_PRODUCT_CATEGORY ( 'part', '', ( #11047 ) ) ;
#5574 = DIRECTION ( 'NONE',  ( -0.8660254037844355990, -0.5000000000000055511, 0.000000000000000000 ) ) ;
#5575 = CARTESIAN_POINT ( 'NONE',  ( 46.49166364869456913, 60.30051614449767072, -4.867452303228181343 ) ) ;
#5576 = CARTESIAN_POINT ( 'NONE',  ( 2.000000000000000000, -1.329782007511007169, -0.7677499999999988223 ) ) ;
#5577 = FACE_OUTER_BOUND ( 'NONE', #3870, .T. ) ;
#5578 = CARTESIAN_POINT ( 'NONE',  ( 7.336184427528458230, 0.000000000000000000, 0.000000000000000000 ) ) ;
#5579 = CARTESIAN_POINT ( 'NONE',  ( 55.08986747509847248, 47.79948385550240886, -3.727524721679197572 ) ) ;
#5580 = VECTOR ( 'NONE', #9165, 999.9999999999998863 ) ;
#5581 = CARTESIAN_POINT ( 'NONE',  ( -0.5000000000000000000, -6.429618962271402616, -1.000000000000000000 ) ) ;
#5582 = ORIENTED_EDGE ( 'NONE', *, *, #6250, .F. ) ;
#5583 = ORIENTED_EDGE ( 'NONE', *, *, #10588, .T. ) ;
#5584 = ORIENTED_EDGE ( 'NONE', *, *, #7033, .F. ) ;
#5585 = DIRECTION ( 'NONE',  ( 0.000000000000000000, 0.000000000000000000, -1.000000000000000000 ) ) ;
#5586 = CARTESIAN_POINT ( 'NONE',  ( -0.9999999999999995559, -15.10102051443364246, 9.000000000000000000 ) ) ;
#5587 = CARTESIAN_POINT ( 'NONE',  ( 7.499999999999834799, -7.009618943233325794, -9.000000000000000000 ) ) ;
#5588 = SURFACE_STYLE_USAGE ( .BOTH. , #10761 ) ;
#5589 = CARTESIAN_POINT ( 'NONE',  ( -14.99999999999999645, -20.00000000000005329, -9.000000000000000000 ) ) ;
#5590 = DIRECTION ( 'NONE',  ( 0.000000000000000000, 1.000000000000000000, 0.000000000000000000 ) ) ;
#5591 = EDGE_CURVE ( 'NONE', #11391, #5893, #8655, .T. ) ;
#5592 = CARTESIAN_POINT ( 'NONE',  ( 50.02271294988512551, 52.49948385550240459, 7.000000000000000888 ) ) ;
#5593 = VECTOR ( 'NONE', #11208, 1000.000000000000000 ) ;
#5594 = CARTESIAN_POINT ( 'NONE',  ( 45.86712807150329496, 51.70051614449766220, 5.649768623646139964 ) ) ;
#5595 = LINE ( 'NONE', #1279, #9504 ) ;
#5596 = CARTESIAN_POINT ( 'NONE',  ( 52.29715082351547295, 54.39948385550239607, 6.992620115222774047 ) ) ;
#5597 = VECTOR ( 'NONE', #6725, 1000.000000000000000 ) ;
#5598 = CARTESIAN_POINT ( 'NONE',  ( 45.31609314410967926, 62.69948385550240744, 6.485486291978119766 ) ) ;
#5599 = EDGE_CURVE ( 'NONE', #1824, #8657, #9536, .T. ) ;
#5600 = ORIENTED_EDGE ( 'NONE', *, *, #11336, .T. ) ;
#5601 = EDGE_LOOP ( 'NONE', ( #1734, #390, #9539, #311 ) ) ;
#5602 = EDGE_LOOP ( 'NONE', ( #13310, #8114, #8277, #6012, #12739 ) ) ;
#5603 = EDGE_CURVE ( 'NONE', #2789, #2711, #10833, .T. ) ;
#5604 = CARTESIAN_POINT ( 'NONE',  ( 2.449293598294706513E-15, -20.00000000000000000, 9.000000000000000000 ) ) ;
#5605 = EDGE_CURVE ( 'NONE', #13041, #8373, #3379, .T. ) ;
#5606 = CARTESIAN_POINT ( 'NONE',  ( 0.3126073911696408136, 2.020725942163688060, 3.500000000000000000 ) ) ;
#5607 = CARTESIAN_POINT ( 'NONE',  ( 43.69122665457040000, 54.00051614449765935, -0.02388180880515696977 ) ) ;
#5608 = DIRECTION ( 'NONE',  ( -0.000000000000000000, -0.000000000000000000, -1.000000000000000000 ) ) ;
#5609 = CARTESIAN_POINT ( 'NONE',  ( 49.97728705011486738, 55.49948385550241170, -8.000000000000001776 ) ) ;
#5610 = CARTESIAN_POINT ( 'NONE',  ( 52.25172492374522903, 57.59948385550241312, -7.007379884777225953 ) ) ;
#5611 = CARTESIAN_POINT ( 'NONE',  ( 5.599999999999999645, 2.020725942163686284, -3.499999999999999556 ) ) ;
#5612 = CARTESIAN_POINT ( 'NONE',  ( 41.58830220609386430, 60.00051614449765935, -0.02388180880514929535 ) ) ;
#5613 = ORIENTED_EDGE ( 'NONE', *, *, #4576, .F. ) ;
#5614 = EDGE_LOOP ( 'NONE', ( #9870, #4992, #7760, #4731 ) ) ;
#5615 = ORIENTED_EDGE ( 'NONE', *, *, #2714, .T. ) ;
#5616 = ORIENTED_EDGE ( 'NONE', *, *, #7461, .T. ) ;
#5617 = EDGE_CURVE ( 'NONE', #686, #2319, #3447, .T. ) ;
#5618 = PLANE ( 'NONE',  #6275 ) ;
#5619 = CARTESIAN_POINT ( 'NONE',  ( 53.50000000000000000, 4.052968581778165278E-16, -3.309499999999999886 ) ) ;
#5620 = EDGE_CURVE ( 'NONE', #11251, #11948, #7771, .T. ) ;
#5621 = AXIS2_PLACEMENT_3D ( 'NONE', #10527, #9560, #9626 ) ;
#5622 = DIRECTION ( 'NONE',  ( -1.000000000000000000, -0.000000000000000000, -0.000000000000000000 ) ) ;
#5623 = MANIFOLD_SOLID_BREP ( 'FlangeHexFillet', #11330 ) ;
#5624 = CARTESIAN_POINT ( 'NONE',  ( 53.54508667620428497, 56.29948385550240886, 4.840751629271157874 ) ) ;
#5625 = CARTESIAN_POINT ( 'NONE',  ( 50.02271294988505446, 48.50051614449765935, -7.000000000000000888 ) ) ;
#5626 = CIRCLE ( 'NONE', #3193, 4.999999999999999112 ) ;
#5627 = CARTESIAN_POINT ( 'NONE',  ( 57.61547081786810764, 50.90051614449765793, -2.450534656007114176 ) ) ;
#5628 = CARTESIAN_POINT ( 'NONE',  ( -0.9999999999999976685, -20.00000000000000000, 8.999999999999998224 ) ) ;
#5629 = CARTESIAN_POINT ( 'NONE',  ( 2.449293598294706513E-15, -20.00000000000000000, -9.000000000000000000 ) ) ;
#5630 = VECTOR ( 'NONE', #9332, 1000.000000000000000 ) ;
#5631 = CARTESIAN_POINT ( 'NONE',  ( 52.29715082351538769, 60.60051614449764656, -6.992620115222796251 ) ) ;
#5632 = AXIS2_PLACEMENT_3D ( 'NONE', #12910, #12975, #9746 ) ;
#5633 = EDGE_LOOP ( 'NONE', ( #10769, #3055, #212, #10386, #5810, #5097, #11215, #7977, #12189, #6524 ) ) ;
#5634 = DIRECTION ( 'NONE',  ( -0.000000000000000000, -0.000000000000000000, 1.000000000000000000 ) ) ;
#5635 = AXIS2_PLACEMENT_3D ( 'NONE', #1061, #13585, #5039 ) ;
#5636 = ORIENTED_EDGE ( 'NONE', *, *, #587, .T. ) ;
#5637 = FACE_OUTER_BOUND ( 'NONE', #11689, .T. ) ;
#5638 = EDGE_CURVE ( 'NONE', #10104, #3586, #5951, .T. ) ;
#5639 = ADVANCED_FACE ( 'NONE', ( #10641 ), #129, .T. ) ;
#5640 = CARTESIAN_POINT ( 'NONE',  ( -1.250000000000000000, -6.429618962271402616, 0.000000000000000000 ) ) ;
#5641 = CARTESIAN_POINT ( 'NONE',  ( 6.242789945155967857, 0.9948955795114693412, 5.105232858000414708 ) ) ;
#5642 = CARTESIAN_POINT ( 'NONE',  ( 0.000000000000000000, 0.000000000000000000, 0.000000000000000000 ) ) ;
#5643 = CARTESIAN_POINT ( 'NONE',  ( 45.90387839640214196, 58.69948385550240033, 5.676469297603166098 ) ) ;
#5644 = B_SPLINE_CURVE_WITH_KNOTS ( 'NONE', 3,
 ( #6421, #8212, #10345, #13509, #4059 ),
 .UNSPECIFIED., .F., .F.,
 ( 4, 1, 4 ),
 ( 0.000000000000000000, 0.002020725942163690506, 0.004041451884327381013 ),
 .UNSPECIFIED. ) ;
#5645 = CARTESIAN_POINT ( 'NONE',  ( 55.11794222512599362, 56.80051614449764941, -3.688883143319583446 ) ) ;
#5646 = CARTESIAN_POINT ( 'NONE',  ( 4.175572532730931208, -2.061029303918052946, 3.569807470274390493 ) ) ;
#5647 = FACE_OUTER_BOUND ( 'NONE', #13076, .T. ) ;
#5648 = MANIFOLD_SOLID_BREP ( 'Cavity1', #3168 ) ;
#5649 = SURFACE_SIDE_STYLE ('',( #10623 ) ) ;
#5650 = CARTESIAN_POINT ( 'NONE',  ( 49.97728705011488870, 47.49948385550240459, -6.000000000000000888 ) ) ;
#5651 = CARTESIAN_POINT ( 'NONE',  ( 4.101954839143059139, -2.368264730582948285, -3.681130640444269631 ) ) ;
#5652 = VERTEX_POINT ( 'NONE', #9868 ) ;
#5653 = EDGE_LOOP ( 'NONE', ( #8541, #8558, #11660, #6376 ) ) ;
#5654 = ORIENTED_EDGE ( 'NONE', *, *, #1220, .T. ) ;
#5655 = LINE ( 'NONE', #11307, #5280 ) ;
#5656 = CARTESIAN_POINT ( 'NONE',  ( 2.725741868436127202, -3.045094352033990148, -3.220599429844051453 ) ) ;
#5657 = DIRECTION ( 'NONE',  ( -0.9396926207859138680, 0.000000000000000000, -0.3420201433256536139 ) ) ;
#5658 = SURFACE_STYLE_FILL_AREA ( #1686 ) ;
#5659 = CARTESIAN_POINT ( 'NONE',  ( 6.507056315241515954, 5.826803161468471437, -0.09231912136634902455 ) ) ;
#5660 = CARTESIAN_POINT ( 'NONE',  ( 2.449293598294706513E-15, -20.00000000000000000, -20.00000000000000000 ) ) ;
#5661 = CARTESIAN_POINT ( 'NONE',  ( 43.33558569842706021, 51.90051614449765793, 2.141517661632167169 ) ) ;
#5662 = LINE ( 'NONE', #6505, #7511 ) ;
#5663 = ADVANCED_FACE ( 'NONE', ( #5937 ), #3312, .F. ) ;
#5664 = CARTESIAN_POINT ( 'NONE',  ( 52.29715082351547295, 52.39948385550241738, 6.992620115222774047 ) ) ;
#5665 = CARTESIAN_POINT ( 'NONE',  ( 42.63976443033212860, 46.99948385550240459, 0.02388180880522514787 ) ) ;
#5666 = CIRCLE ( 'NONE', #4553, 3.500000000000000000 ) ;
#5667 = CARTESIAN_POINT ( 'NONE',  ( 49.97728705011486738, 65.49948385550240459, -8.000000000000001776 ) ) ;
#5668 = ORIENTED_EDGE ( 'NONE', *, *, #11597, .T. ) ;
#5669 = ORIENTED_EDGE ( 'NONE', *, *, #4640, .F. ) ;
#5670 = CARTESIAN_POINT ( 'NONE',  ( 4.030859730899086557, -1.403482646610860307, -3.500000000000000000 ) ) ;
#5671 = EDGE_LOOP ( 'NONE', ( #1487, #1663, #4064, #2001 ) ) ;
#5672 = CARTESIAN_POINT ( 'NONE',  ( 0.1388410611046073107, 2.351840044243033834, -2.926493552096022022 ) ) ;
#5673 = APPLICATION_CONTEXT ( 'automotive_design' ) ;
#5674 = CARTESIAN_POINT ( 'NONE',  ( 0.000000000000000000, 0.000000000000000000, -4.000000000000000000 ) ) ;
#5675 = AXIS2_PLACEMENT_3D ( 'NONE', #4223, #3256, #12445 ) ;
#5676 = CARTESIAN_POINT ( 'NONE',  ( 43.69122665457040000, 52.00051614449766646, -0.02388180880515696977 ) ) ;
#5677 = PLANE ( 'NONE',  #5548 ) ;
#5678 = CARTESIAN_POINT ( 'NONE',  ( 58.41169779390614281, 55.99948385550241170, -0.02388180880523160798 ) ) ;
#5679 = CARTESIAN_POINT ( 'NONE',  ( 47.74827507625478518, 58.59948385550238470, 7.007379884777227730 ) ) ;
#5680 = CARTESIAN_POINT ( 'NONE',  ( 4.151274195509681242, -4.079825909417492902, 4.401844587977598791E-16 ) ) ;
#5681 = ADVANCED_FACE ( 'NONE', ( #12018 ), #12542, .T. ) ;
#5682 = CARTESIAN_POINT ( 'NONE',  ( 45.27934281921082516, 63.70051614449766930, 6.458785618021089192 ) ) ;
#5683 = EDGE_CURVE ( 'NONE', #2414, #8791, #5282, .T. ) ;
#5684 = PRODUCT_DEFINITION_SHAPE ( 'NONE', 'NONE',  #13663 ) ;
#5685 = ORIENTED_EDGE ( 'NONE', *, *, #12292, .T. ) ;
#5686 = ORIENTED_EDGE ( 'NONE', *, *, #6210, .T. ) ;
#5687 = VERTEX_POINT ( 'NONE', #3867 ) ;
#5688 = ORIENTED_EDGE ( 'NONE', *, *, #7053, .T. ) ;
#5689 = CARTESIAN_POINT ( 'NONE',  ( 50.00000000000000000, 40.00000000000000000, 0.000000000000000000 ) ) ;
#5690 = CARTESIAN_POINT ( 'NONE',  ( 6.165086708099361879, -6.325508935188243420, 9.000000000000000000 ) ) ;
#5691 = DIRECTION ( 'NONE',  ( 0.000000000000000000, 0.000000000000000000, 1.000000000000000000 ) ) ;
#5692 = CARTESIAN_POINT ( 'NONE',  ( -74.99999999999998579, 7.499999999999975131, -10.00000000000000000 ) ) ;
#5693 = CARTESIAN_POINT ( 'NONE',  ( 53.50833635130540955, 53.69948385550240744, -4.867452303228209765 ) ) ;
#5694 = CARTESIAN_POINT ( 'NONE',  ( 55.94051828345054389, 47.20051614449766220, 4.345558710429044957 ) ) ;
#5695 = CARTESIAN_POINT ( 'NONE',  ( 43.20883090819742023, 52.20051614449766220, -4.963592699178938972 ) ) ;
#5696 = ADVANCED_BREP_SHAPE_REPRESENTATION ( '', ( #10159, #430 ), #11706 ) ;
#5697 = DIRECTION ( 'NONE',  ( 0.000000000000000000, 0.000000000000000000, 1.000000000000000000 ) ) ;
#5698 = DIRECTION ( 'NONE',  ( -0.5000000000000061062, 1.060575238724902601E-16, -0.8660254037844351549 ) ) ;
#5699 = EDGE_CURVE ( 'NONE', #10200, #7846, #1958, .T. ) ;
#5700 = CARTESIAN_POINT ( 'NONE',  ( 52.62207051974829852, 44.60051614449766078, -7.992620115222797139 ) ) ;
#5701 = EDGE_CURVE ( 'NONE', #12678, #757, #3502, .T. ) ;
#5702 = ORIENTED_EDGE ( 'NONE', *, *, #10572, .F. ) ;
#5703 = LINE ( 'NONE', #8806, #1290 ) ;
#5704 = EDGE_CURVE ( 'NONE', #12356, #5390, #1160, .T. ) ;
#5705 = ORIENTED_EDGE ( 'NONE', *, *, #12012, .F. ) ;
#5706 = CARTESIAN_POINT ( 'NONE',  ( 1.000000000000002442, -20.00000000000000000, 8.999999999999998224 ) ) ;
#5707 = CARTESIAN_POINT ( 'NONE',  ( 6.390983631292896483, 3.014665224428355383, 4.999999999999999112 ) ) ;
#5708 = DIRECTION ( 'NONE',  ( 1.000000000000000000, 0.000000000000000000, 0.000000000000000000 ) ) ;
#5709 = CARTESIAN_POINT ( 'NONE',  ( 47.74827507625478518, 56.59948385550238470, 7.007379884777227730 ) ) ;
#5710 = AXIS2_PLACEMENT_3D ( 'NONE', #3944, #13330, #13398 ) ;
#5711 = CARTESIAN_POINT ( 'NONE',  ( 48.02776887271750184, 55.60051614449765367, 5.992620115222795363 ) ) ;
#5712 = CARTESIAN_POINT ( 'NONE',  ( -2.500000000000000444, 3.061616997868383634E-16, -5.000000000000000888 ) ) ;
#5713 = CARTESIAN_POINT ( 'NONE',  ( 0.8816464618332836567, -24.71833652004169934, 9.999999999999998224 ) ) ;
#5714 = MANIFOLD_SOLID_BREP ( 'EndChamfer', #7149 ) ;
#5715 = CARTESIAN_POINT ( 'NONE',  ( 43.69122665457040000, 64.00051614449765225, -0.02388180880515696977 ) ) ;
#5716 = CARTESIAN_POINT ( 'NONE',  ( 44.05948171654949874, 64.79948385550240175, 4.345558710429105354 ) ) ;
#5717 = CARTESIAN_POINT ( 'NONE',  ( -11.49038105676659249, -12.50000000000003020, -9.000000000000000000 ) ) ;
#5718 = EDGE_LOOP ( 'NONE', ( #8915, #4138, #9379, #5012 ) ) ;
#5719 = VECTOR ( 'NONE', #4978, 1000.000000000000000 ) ;
#5720 = ORIENTED_EDGE ( 'NONE', *, *, #3130, .F. ) ;
#5721 = DIRECTION ( 'NONE',  ( 0.000000000000000000, 0.000000000000000000, -1.000000000000000000 ) ) ;
#5722 = AXIS2_PLACEMENT_3D ( 'NONE', #1331, #6490, #12884 ) ;
#5723 = B_SPLINE_CURVE_WITH_KNOTS ( 'NONE', 3,
 ( #5740, #2681, #9120, #12088, #9941, #11113 ),
 .UNSPECIFIED., .F., .F.,
 ( 4, 2, 4 ),
 ( 4.336808689942017736E-19, 0.001488912493401929995, 0.002977824986803859555 ),
 .UNSPECIFIED. ) ;
#5724 = CARTESIAN_POINT ( 'NONE',  ( -20.00000000000000000, -19.99999999999999289, -23.00000000000000000 ) ) ;
#5725 = CARTESIAN_POINT ( 'NONE',  ( 3.973110223765528914, 0.6902454861566579281, -3.565797985667391146 ) ) ;
#5726 =( LENGTH_UNIT ( ) NAMED_UNIT ( * ) SI_UNIT ( .MILLI., .METRE. ) );
#5727 = CARTESIAN_POINT ( 'NONE',  ( 6.357976367241986893, 5.421935536069748096, 0.8264656814052228073 ) ) ;
#5728 = CARTESIAN_POINT ( 'NONE',  ( 5.599999999999999645, 3.061616997868383634E-16, -2.500000000000000444 ) ) ;
#5729 = CARTESIAN_POINT ( 'NONE',  ( 43.34962307344078880, 56.10051614449766078, -2.184720259617096705 ) ) ;
#5730 = AXIS2_PLACEMENT_3D ( 'NONE', #3152, #10543, #1051 ) ;
#5731 = FACE_OUTER_BOUND ( 'NONE', #12870, .T. ) ;
#5732 = CARTESIAN_POINT ( 'NONE',  ( 44.05948171654949874, 50.79948385550238754, 4.345558710429105354 ) ) ;
#5733 = AXIS2_PLACEMENT_3D ( 'NONE', #6951, #5918, #12198 ) ;
#5734 = CARTESIAN_POINT ( 'NONE',  ( 50.02271294988513972, 62.49948385550240459, 8.000000000000001776 ) ) ;
#5735 = ORIENTED_EDGE ( 'NONE', *, *, #325, .T. ) ;
#5736 = VERTEX_POINT ( 'NONE', #2378 ) ;
#5737 = PRESENTATION_LAYER_ASSIGNMENT (  '', '', ( #8604 ) ) ;
#5738 = CARTESIAN_POINT ( 'NONE',  ( 3.880198502136737115, 0.7307680362927179152, -3.499999999999999556 ) ) ;
#5739 = VERTEX_POINT ( 'NONE', #4534 ) ;
#5740 = CARTESIAN_POINT ( 'NONE',  ( 6.534838248920899595, -2.951765777552420644, -5.112608298763837489 ) ) ;
#5741 = EDGE_CURVE ( 'NONE', #8082, #822, #7275, .T. ) ;
#5742 = CARTESIAN_POINT ( 'NONE',  ( 45.15499999999999403, 0.000000000000000000, 0.000000000000000000 ) ) ;
#5743 = CARTESIAN_POINT ( 'NONE',  ( 51.97223112728249816, 54.60051614449766788, -5.992620115222793586 ) ) ;
#5744 = DIRECTION ( 'NONE',  ( 9.858538378746663627E-23, -5.031452844637890958E-23, 1.000000000000000000 ) ) ;
#5745 = VECTOR ( 'NONE', #3207, 1000.000000000000000 ) ;
#5746 = CARTESIAN_POINT ( 'NONE',  ( 57.60143344285433642, 51.89948385550241028, -2.493737253992118319 ) ) ;
#5747 = CIRCLE ( 'NONE', #4419, 1.500000000000000666 ) ;
#5748 = CARTESIAN_POINT ( 'NONE',  ( 49.97728705011488159, 57.49948385550241170, -7.000000000000000888 ) ) ;
#5749 = CARTESIAN_POINT ( 'NONE',  ( -4.211140560182196957, 2.431303136016537803, -3.745885042887433514 ) ) ;
#5750 = CARTESIAN_POINT ( 'NONE',  ( 50.02271294988505446, 62.50051614449767357, -8.000000000000001776 ) ) ;
#5751 = EDGE_LOOP ( 'NONE', ( #12578, #9469, #9453, #4431, #9188, #2556, #12003, #3500 ) ) ;
#5752 = CONTEXT_DEPENDENT_SHAPE_REPRESENTATION ( #7793, #11965 ) ;
#5753 = ORIENTED_EDGE ( 'NONE', *, *, #2913, .F. ) ;
#5754 = ORIENTED_EDGE ( 'NONE', *, *, #846, .F. ) ;
#5755 = ORIENTED_EDGE ( 'NONE', *, *, #3985, .F. ) ;
#5756 = CARTESIAN_POINT ( 'NONE',  ( 6.355827204229362870, 5.411702751981843917, -0.8440485055075606091 ) ) ;
#5757 = STYLED_ITEM ( 'NONE', ( #2421 ), #5696 ) ;
#5759 = TOROIDAL_SURFACE ( 'NONE', #13459, 5.384454397937118664, 0.5155456020628804703 ) ;
#5758 = CARTESIAN_POINT ( 'NONE',  ( 75.00000000000002842, -39.99999999999998579, 10.00000000000000000 ) ) ;
#5760 = FILL_AREA_STYLE ('',( #8734 ) ) ;
#5761 = CARTESIAN_POINT ( 'NONE',  ( 0.04320752586819863461, 0.9836842030436160345, 4.999999999999999112 ) ) ;
#5762 = CARTESIAN_POINT ( 'NONE',  ( 0.04201760816083378175, -0.9730571234388133428, 4.999999999999997335 ) ) ;
#5763 = CARTESIAN_POINT ( 'NONE',  ( 46.49166364869460466, 54.69948385550240033, 4.867452303228209765 ) ) ;
#5764 = CARTESIAN_POINT ( 'NONE',  ( 45.86712807150329496, 47.70051614449766220, 5.649768623646139964 ) ) ;
#5765 = CARTESIAN_POINT ( 'NONE',  ( 47.37792948025170858, 51.60051614449766788, 7.992620115222797139 ) ) ;
#5766 = PLANE ( 'NONE',  #12835 ) ;
#5767 = FACE_OUTER_BOUND ( 'NONE', #2473, .T. ) ;
#5768 = EDGE_CURVE ( 'NONE', #3586, #13062, #13355, .T. ) ;
#5769 = CARTESIAN_POINT ( 'NONE',  ( 44.03140696652198471, 63.80051614449765651, 4.306917132069485454 ) ) ;
#5770 = AXIS2_PLACEMENT_3D ( 'NONE', #603, #7138, #4786 ) ;
#5771 = EDGE_LOOP ( 'NONE', ( #7058, #9758 ) ) ;
#5772 = DIRECTION ( 'NONE',  ( -0.000000000000000000, -0.000000000000000000, 1.000000000000000000 ) ) ;
#5773 = EDGE_CURVE ( 'NONE', #3318, #8372, #6391, .T. ) ;
#5774 = ORIENTED_EDGE ( 'NONE', *, *, #11276, .F. ) ;
#5775 = CARTESIAN_POINT ( 'NONE',  ( -14.14213562373094568, -25.00000000000000000, -20.00000000000000000 ) ) ;
#5776 = CARTESIAN_POINT ( 'NONE',  ( 4.030867648404857562, -3.732851566702167556, -0.5345114293585713217 ) ) ;
#5777 = ADVANCED_FACE ( 'NONE', ( #11657 ), #2170, .F. ) ;
#5778 = VECTOR ( 'NONE', #6965, 1000.000000000000000 ) ;
#5779 = EDGE_CURVE ( 'NONE', #6035, #9307, #2395, .T. ) ;
#5780 = CARTESIAN_POINT ( 'NONE',  ( -62.49999999999997158, 32.50000000000001421, -20.00000000000000000 ) ) ;
#5781 = CARTESIAN_POINT ( 'NONE',  ( 45.90387839640214196, 54.69948385550240744, 5.676469297603166098 ) ) ;
#5782 = CARTESIAN_POINT ( 'NONE',  ( 51.92680522751238925, 57.40051614449767214, 6.007379884777208190 ) ) ;
#5783 = LINE ( 'NONE', #6877, #6989 ) ;
#5784 = FACE_OUTER_BOUND ( 'NONE', #2199, .T. ) ;
#5785 = MANIFOLD_SOLID_BREP ( 'M4 Clearance Hole1', #2950 ) ;
#5786 = CARTESIAN_POINT ( 'NONE',  ( 49.97728705011494554, 61.50051614449766646, 6.000000000000000888 ) ) ;
#5787 = CARTESIAN_POINT ( 'NONE',  ( 51.92680522751233951, 45.59948385550240602, -6.007379884777223289 ) ) ;
#5788 = CARTESIAN_POINT ( 'NONE',  ( -62.49999999999997158, 45.00000000000001421, -15.00000000000000000 ) ) ;
#5789 = ORIENTED_EDGE ( 'NONE', *, *, #3217, .T. ) ;
#5790 = AXIS2_PLACEMENT_3D ( 'NONE', #2428, #13073, #483 ) ;
#5791 = UNCERTAINTY_MEASURE_WITH_UNIT (LENGTH_MEASURE( 1.000000000000000082E-05 ), #4751, 'distance_accuracy_value', 'NONE');
#5792 = ORIENTED_EDGE ( 'NONE', *, *, #8609, .F. ) ;
#5793 = CYLINDRICAL_SURFACE ( 'NONE', #12977, 1.500000000000000444 ) ;
#5794 = DIRECTION ( 'NONE',  ( 0.000000000000000000, 0.000000000000000000, 1.000000000000000000 ) ) ;
#5795 = CARTESIAN_POINT ( 'NONE',  ( -9.999999999999998224, 15.00000000000001776, 15.00000000000000000 ) ) ;
#5796 = SHAPE_REPRESENTATION_RELATIONSHIP ( 'NONE' , 'NONE' ,  #11930, #8490 ) ;
#5797 = FACE_BOUND ( 'NONE', #5771, .T. ) ;
#5798 = AXIS2_PLACEMENT_3D ( 'NONE', #914, #6341, #5092 ) ;
#5799 = CARTESIAN_POINT ( 'NONE',  ( 56.66441430157294690, 62.90051614449765083, -2.141517661632166281 ) ) ;
#5800 = CARTESIAN_POINT ( 'NONE',  ( 2.000000000000000000, 0.8865213383406715941, 1.535499999999999199 ) ) ;
#5801 = CIRCLE ( 'NONE', #11303, 0.7500000000000000000 ) ;
#5802 = DIRECTION ( 'NONE',  ( 0.000000000000000000, 0.000000000000000000, 1.000000000000000000 ) ) ;
#5803 = CARTESIAN_POINT ( 'NONE',  ( 57.36023556966787851, 49.99948385550238328, -0.02388180880522424582 ) ) ;
#5804 = CARTESIAN_POINT ( 'NONE',  ( 56.66441430157296821, 46.09948385550240602, 2.141517661632100111 ) ) ;
#5805 = EDGE_CURVE ( 'NONE', #8730, #9809, #12556, .T. ) ;
#5806 = CARTESIAN_POINT ( 'NONE',  ( 42.39856655714566358, 62.89948385550240317, 2.493737253992119207 ) ) ;
#5807 = ORIENTED_EDGE ( 'NONE', *, *, #4715, .F. ) ;
#5808 = ORIENTED_EDGE ( 'NONE', *, *, #13277, .F. ) ;
#5809 = CARTESIAN_POINT ( 'NONE',  ( 4.180232103119976728, 2.085387772176679366, -3.570466442734698820 ) ) ;
#5810 = ORIENTED_EDGE ( 'NONE', *, *, #8070, .T. ) ;
#5811 = CARTESIAN_POINT ( 'NONE',  ( -2.919722569185572480E-15, 2.859595677584338524, -2.047034997319574945 ) ) ;
#5812 = AXIS2_PLACEMENT_3D ( 'NONE', #3682, #13002, #1589 ) ;
#5813 = CARTESIAN_POINT ( 'NONE',  ( -7.499999999999923617, -32.99038105676662269, -9.000000000000000000 ) ) ;
#5814 = CARTESIAN_POINT ( 'NONE',  ( 55.08986747509849380, 55.20051614449766220, 3.727524721679155384 ) ) ;
#5815 = VECTOR ( 'NONE', #1102, 1000.000000000000000 ) ;
#5816 = CARTESIAN_POINT ( 'NONE',  ( 6.196878017913833858, 5.292377467571573568, 0.8333333333333322601 ) ) ;
#5817 = CARTESIAN_POINT ( 'NONE',  ( 56.81924384183011512, 54.19948385550241454, 4.924951120819313743 ) ) ;
#5818 = CARTESIAN_POINT ( 'NONE',  ( 50.02271294988512551, 58.49948385550241170, 7.000000000000000888 ) ) ;
#5819 = FACE_OUTER_BOUND ( 'NONE', #9398, .T. ) ;
#5820 = CARTESIAN_POINT ( 'NONE',  ( 45.31609314410967926, 46.69948385550240744, 6.485486291978119766 ) ) ;
#5821 = AXIS2_PLACEMENT_3D ( 'NONE', #6845, #13185, #11120 ) ;
#5822 = VERTEX_POINT ( 'NONE', #6004 ) ;
#5823 = VERTEX_POINT ( 'NONE', #10204 ) ;
#5824 = ORIENTED_EDGE ( 'NONE', *, *, #3992, .F. ) ;
#5825 = ORIENTED_EDGE ( 'NONE', *, *, #427, .F. ) ;
#5826 = VECTOR ( 'NONE', #4649, 1000.000000000000000 ) ;
#5827 = FACE_OUTER_BOUND ( 'NONE', #7940, .T. ) ;
#5828 = CARTESIAN_POINT ( 'NONE',  ( 0.000000000000000000, 0.000000000000000000, 0.000000000000000000 ) ) ;
#5829 = DIRECTION ( 'NONE',  ( 0.000000000000000000, -0.000000000000000000, 1.000000000000000000 ) ) ;
#5830 = CARTESIAN_POINT ( 'NONE',  ( -6.259644161404860030E-16, -4.618802153517027165, -3.433295621305388234 ) ) ;
#5831 = CARTESIAN_POINT ( 'NONE',  ( -8.759913291900394583, -32.17636723815387256, -9.000000000000000000 ) ) ;
#5832 = CARTESIAN_POINT ( 'NONE',  ( 55.08986747509847248, 55.79948385550239465, -3.727524721679197572 ) ) ;
#5833 = DIRECTION ( 'NONE',  ( -0.7779254092217071648, -0.6283566325640553840, 0.000000000000000000 ) ) ;
#5834 = CARTESIAN_POINT ( 'NONE',  ( 54.72065718078918906, 52.70051614449766220, -6.458785618021089192 ) ) ;
#5835 = CYLINDRICAL_SURFACE ( 'NONE', #13071, 4.799999999999999822 ) ;
#5836 = CARTESIAN_POINT ( 'NONE',  ( 45.86712807150329496, 63.70051614449766220, 5.649768623646139964 ) ) ;
#5837 = ORIENTED_EDGE ( 'NONE', *, *, #360, .F. ) ;
#5838 = DIRECTION ( 'NONE',  ( 1.000000000000000000, 0.000000000000000000, 0.000000000000000000 ) ) ;
#5839 = EDGE_CURVE ( 'NONE', #2590, #9688, #3088, .T. ) ;
#5840 = VECTOR ( 'NONE', #1973, 1000.000000000000000 ) ;
#5841 = ORIENTED_EDGE ( 'NONE', *, *, #10069, .T. ) ;
#5842 = DIRECTION ( 'NONE',  ( 0.000000000000000000, 0.000000000000000000, 1.000000000000000000 ) ) ;
#5843 = AXIS2_PLACEMENT_3D ( 'NONE', #12475, #11440, #13497 ) ;
#5844 = DIRECTION ( 'NONE',  ( -9.858538378746663627E-23, 5.031452844637890958E-23, -1.000000000000000000 ) ) ;
#5845 = CARTESIAN_POINT ( 'NONE',  ( 56.66441430157296821, 58.09948385550240602, 2.141517661632100111 ) ) ;
#5846 = CARTESIAN_POINT ( 'NONE',  ( 43.33558569842703179, 53.09948385550240602, -2.141517661632099223 ) ) ;
#5847 = AXIS2_PLACEMENT_3D ( 'NONE', #3032, #7259, #7333 ) ;
#5848 = SHAPE_REPRESENTATION ( 'hex flange bolt small_iso_ISO 4162 - M5 x 40 x 16-N', ( #430 ), #9694 ) ;
#5849 = CARTESIAN_POINT ( 'NONE',  ( 2.449293598294706513E-15, -5.000000000000000888, 9.000000000000000000 ) ) ;
#5850 = ADVANCED_FACE ( 'NONE', ( #854 ), #4837, .T. ) ;
#5851 = CIRCLE ( 'NONE', #5412, 15.00000000000000000 ) ;
#5852 = DIRECTION ( 'NONE',  ( -0.000000000000000000, -0.000000000000000000, -1.000000000000000000 ) ) ;
#5853 = DIRECTION ( 'NONE',  ( 0.000000000000000000, 0.000000000000000000, 1.000000000000000000 ) ) ;
#5854 = CARTESIAN_POINT ( 'NONE',  ( 44.91013252490150620, 64.20051614449766930, -3.727524721679154940 ) ) ;
#5855 = CARTESIAN_POINT ( 'NONE',  ( 44.28664221472220675, 47.09948385550240602, -1.832500667257165317 ) ) ;
#5856 = LINE ( 'NONE', #1678, #4512 ) ;
#5857 = EDGE_CURVE ( 'NONE', #13447, #6557, #3943, .T. ) ;
#5858 = ORIENTED_EDGE ( 'NONE', *, *, #5211, .F. ) ;
#5859 = VECTOR ( 'NONE', #11174, 1000.000000000000000 ) ;
#5860 = EDGE_CURVE ( 'NONE', #11777, #7974, #11530, .T. ) ;
#5861 = ORIENTED_EDGE ( 'NONE', *, *, #10696, .F. ) ;
#5862 = ORIENTED_EDGE ( 'NONE', *, *, #4489, .T. ) ;
#5863 = LINE ( 'NONE', #13226, #4825 ) ;
#5864 = VECTOR ( 'NONE', #3386, 1000.000000000000000 ) ;
#5865 = DIRECTION ( 'NONE',  ( 0.000000000000000000, 0.000000000000000000, -1.000000000000000000 ) ) ;
#5866 = DIRECTION ( 'NONE',  ( -1.000000000000000000, 0.000000000000000000, 0.000000000000000000 ) ) ;
#5867 = CARTESIAN_POINT ( 'NONE',  ( 6.242800618755108388, 4.918813924286816963, 1.690830708135752758 ) ) ;
#5868 = DIRECTION ( 'NONE',  ( 0.000000000000000000, 0.000000000000000000, 1.000000000000000000 ) ) ;
#5869 = CARTESIAN_POINT ( 'NONE',  ( 50.02271294988505446, 58.50051614449765935, -7.000000000000000888 ) ) ;
#5870 = CARTESIAN_POINT ( 'NONE',  ( 6.390821132688881967, 3.013780087859769363, -5.000000000000000000 ) ) ;
#5871 = CARTESIAN_POINT ( 'NONE',  ( 3.806834918298644954, 3.031088913245535199, -1.749999999999998446 ) ) ;
#5872 = CARTESIAN_POINT ( 'NONE',  ( 56.65037692655918988, 59.89948385550241028, -2.184720259617163762 ) ) ;
#5873 = CARTESIAN_POINT ( 'NONE',  ( 42.63976443033212860, 46.99948385550240459, 0.02388180880522514787 ) ) ;
#5874 = ORIENTED_EDGE ( 'NONE', *, *, #11247, .T. ) ;
#5875 = VERTEX_POINT ( 'NONE', #11385 ) ;
#5876 = CARTESIAN_POINT ( 'NONE',  ( 1.000000000000002442, -20.00000000000000000, -9.000000000000001776 ) ) ;
#5877 = ORIENTED_EDGE ( 'NONE', *, *, #12263, .F. ) ;
#5878 = CARTESIAN_POINT ( 'NONE',  ( 8.978549240895586059E-17, -0.3420925509381363971, 3.500000000000000444 ) ) ;
#5879 = DIRECTION ( 'NONE',  ( 0.000000000000000000, -0.000000000000000000, 1.000000000000000000 ) ) ;
#5880 = CARTESIAN_POINT ( 'NONE',  ( 56.30877334542961421, 63.00051614449766646, 0.02388180880515774693 ) ) ;
#5881 = PRODUCT_DEFINITION_SHAPE ( 'NONE', 'NONE',  #6587 ) ;
#5882 = CARTESIAN_POINT ( 'NONE',  ( 4.197478902586992966, -0.8524102783748346290, -3.505063281295504041 ) ) ;
#5883 = CARTESIAN_POINT ( 'NONE',  ( 54.72065718078924590, 62.29948385550241596, 6.458785618021043895 ) ) ;
#5884 = CARTESIAN_POINT ( 'NONE',  ( 42.63976443033212860, 60.99948385550238328, 0.02388180880522514787 ) ) ;
#5885 = FACE_BOUND ( 'NONE', #9509, .T. ) ;
#5886 = EDGE_CURVE ( 'NONE', #6144, #967, #10481, .T. ) ;
#5887 = CARTESIAN_POINT ( 'NONE',  ( 49.97728705011486738, 45.49948385550240459, -8.000000000000001776 ) ) ;
#5888 = VERTEX_POINT ( 'NONE', #3844 ) ;
#5889 = ITEM_DEFINED_TRANSFORMATION ( 'NONE', 'NONE', #5309,  #430 ) ;
#5890 = VERTEX_POINT ( 'NONE', #7028 ) ;
#5891 = AXIS2_PLACEMENT_3D ( 'NONE', #1745, #4950, #2583 ) ;
#5892 = VERTEX_POINT ( 'NONE', #713 ) ;
#5893 = VERTEX_POINT ( 'NONE', #8282 ) ;
#5894 = CARTESIAN_POINT ( 'NONE',  ( 8.500000000000000000, 5.773502691896261751, 0.000000000000000000 ) ) ;
#5895 = CARTESIAN_POINT ( 'NONE',  ( 10.00000000000000000, 0.000000000000000000, -9.999999999999998224 ) ) ;
#5896 = LINE ( 'NONE', #8244, #12405 ) ;
#5897 = DIRECTION ( 'NONE',  ( -0.000000000000000000, -0.000000000000000000, -1.000000000000000000 ) ) ;
#5898 = DIRECTION ( 'NONE',  ( -0.000000000000000000, -0.000000000000000000, 1.000000000000000000 ) ) ;
#5899 = CARTESIAN_POINT ( 'NONE',  ( 55.69932041026404335, 63.89948385550240317, -1.875703265242203432 ) ) ;
#5900 = CARTESIAN_POINT ( 'NONE',  ( 55.94051828345054389, 53.20051614449766220, 4.345558710429044957 ) ) ;
#5901 = CARTESIAN_POINT ( 'NONE',  ( 50.02271294988505446, 54.50051614449765935, -8.000000000000001776 ) ) ;
#5902 = CARTESIAN_POINT ( 'NONE',  ( 0.03027795055833727364, 0.6888063905328611902, 3.500000000000000888 ) ) ;
#5903 = CARTESIAN_POINT ( 'NONE',  ( -75.00000000000001421, -2.602085213965211904E-14, 0.000000000000000000 ) ) ;
#5904 = CARTESIAN_POINT ( 'NONE',  ( 54.72065718078918906, 46.70051614449766220, -6.458785618021089192 ) ) ;
#5906 = EDGE_LOOP ( 'NONE', ( #1170, #11863, #4353, #13621, #2400 ) ) ;
#5905 = ORIENTED_EDGE ( 'NONE', *, *, #3479, .T. ) ;
#5907 = CARTESIAN_POINT ( 'NONE',  ( -59.84999999999998721, 32.50000000000001421, 10.00000000000000000 ) ) ;
#5908 = ORIENTED_EDGE ( 'NONE', *, *, #3602, .F. ) ;
#5909 = CARTESIAN_POINT ( 'NONE',  ( 12.17636723815370736, -11.24008670809938693, -9.000000000000000000 ) ) ;
#5910 = PLANE ( 'NONE',  #33 ) ;
#5911 = DIRECTION ( 'NONE',  ( 0.000000000000000000, 0.000000000000000000, 1.000000000000000000 ) ) ;
#5912 = CARTESIAN_POINT ( 'NONE',  ( 55.96859303347804371, 64.19948385550239323, 4.306917132069425946 ) ) ;
#5913 = ADVANCED_FACE ( 'NONE', ( #12279 ), #9361, .T. ) ;
#5914 = CARTESIAN_POINT ( 'NONE',  ( 42.63976443033212149, 60.99948385550239749, 0.02388180880522514787 ) ) ;
#5915 = CARTESIAN_POINT ( 'NONE',  ( 0.02993401039713673023, -2.688325911136453694, 2.343682934607768775 ) ) ;
#5916 = EDGE_CURVE ( 'NONE', #6266, #5253, #3287, .T. ) ;
#5917 = DIRECTION ( 'NONE',  ( 0.000000000000000000, 0.000000000000000000, 1.000000000000000000 ) ) ;
#5918 = DIRECTION ( 'NONE',  ( -0.000000000000000000, -0.000000000000000000, -1.000000000000000000 ) ) ;
#5919 = CARTESIAN_POINT ( 'NONE',  ( 51.97223112728249816, 62.60051614449765367, -5.992620115222793586 ) ) ;
#5920 = CARTESIAN_POINT ( 'NONE',  ( 48.07319477248768180, 54.59948385550240602, 6.007379884777225953 ) ) ;
#5921 = DIRECTION ( 'NONE',  ( 1.000000000000000000, 0.000000000000000000, 0.000000000000000000 ) ) ;
#5922 = ORIENTED_EDGE ( 'NONE', *, *, #3394, .T. ) ;
#5923 = ORIENTED_EDGE ( 'NONE', *, *, #9081, .F. ) ;
#5924 = ORIENTED_EDGE ( 'NONE', *, *, #8072, .T. ) ;
#5925 = DIRECTION ( 'NONE',  ( 0.000000000000000000, 0.000000000000000000, -1.000000000000000000 ) ) ;
#5926 = AXIS2_PLACEMENT_3D ( 'NONE', #11504, #5287, #10391 ) ;
#5927 = DIRECTION ( 'NONE',  ( 1.000000000000000000, 0.000000000000000000, 0.000000000000000000 ) ) ;
#5928 = CARTESIAN_POINT ( 'NONE',  ( 6.506891779418576327, -2.833891091414761032, -5.091556646552826138 ) ) ;
#5929 =( NAMED_UNIT ( * ) SI_UNIT ( $, .STERADIAN. ) SOLID_ANGLE_UNIT ( ) );
#5930 = CYLINDRICAL_SURFACE ( 'NONE', #4230, 2.649999999999985700 ) ;
#5931 = LINE ( 'NONE', #3646, #9541 ) ;
#5932 = CARTESIAN_POINT ( 'NONE',  ( 55.94051828345053679, 57.20051614449766930, 4.345558710429044069 ) ) ;
#5933 = DIRECTION ( 'NONE',  ( -0.000000000000000000, 0.000000000000000000, -1.000000000000000000 ) ) ;
#5934 = CARTESIAN_POINT ( 'NONE',  ( 50.02271294988506156, 48.50051614449765935, -6.000000000000000888 ) ) ;
#5935 = CARTESIAN_POINT ( 'NONE',  ( -1.000000000000000000, -14.00000000000000000, 8.999999999999998224 ) ) ;
#5936 = CARTESIAN_POINT ( 'NONE',  ( 43.34962307344081012, 58.89948385550241028, 2.184720259617164650 ) ) ;
#5937 = FACE_OUTER_BOUND ( 'NONE', #10317, .T. ) ;
#5938 = APPLICATION_CONTEXT ( 'automotive_design' ) ;
#5939 = VECTOR ( 'NONE', #2679, 1000.000000000000000 ) ;
#5940 = EDGE_CURVE ( 'NONE', #11968, #5420, #860, .T. ) ;
#5941 = CARTESIAN_POINT ( 'NONE',  ( 42.63976443033212860, 48.99948385550240459, 0.02388180880522514787 ) ) ;
#5942 = PRESENTATION_LAYER_ASSIGNMENT (  '', '', ( #11294 ) ) ;
#5943 = ORIENTED_EDGE ( 'NONE', *, *, #7215, .T. ) ;
#5944 = ORIENTED_EDGE ( 'NONE', *, *, #13033, .F. ) ;
#5945 = CARTESIAN_POINT ( 'NONE',  ( 4.158921444904715159, -2.089933220600048713, -3.500000000000000000 ) ) ;
#5946 = VERTEX_POINT ( 'NONE', #4199 ) ;
#5947 = CARTESIAN_POINT ( 'NONE',  ( -9.999999999999996447, 25.00000000000001776, 15.00000000000000000 ) ) ;
#5948 = AXIS2_PLACEMENT_3D ( 'NONE', #8746, #8101, #1648 ) ;
#5949 = LINE ( 'NONE', #9123, #207 ) ;
#5950 = EDGE_CURVE ( 'NONE', #10229, #6754, #5382, .T. ) ;
#5951 = CIRCLE ( 'NONE', #4177, 3.500000000000000000 ) ;
#5952 = CARTESIAN_POINT ( 'NONE',  ( 51.92680522751238925, 61.40051614449765793, 6.007379884777208190 ) ) ;
#5953 = EDGE_CURVE ( 'NONE', #12157, #12919, #111, .T. ) ;
#5954 = FACE_OUTER_BOUND ( 'NONE', #969, .T. ) ;
#5955 = CARTESIAN_POINT ( 'NONE',  ( 49.97728705011486738, 59.49948385550240459, -8.000000000000001776 ) ) ;
#5956 = EDGE_CURVE ( 'NONE', #439, #10938, #9254, .T. ) ;
#5957 = CARTESIAN_POINT ( 'NONE',  ( 43.33558569842703179, 61.09948385550240602, -2.141517661632099223 ) ) ;
#5958 = CARTESIAN_POINT ( 'NONE',  ( -22.00000000000000000, -19.99999999999999289, -12.00000000000000000 ) ) ;
#5959 = PRESENTATION_LAYER_ASSIGNMENT (  '', '', ( #8819 ) ) ;
#5960 = CARTESIAN_POINT ( 'NONE',  ( 57.60143344285433642, 47.89948385550240317, -2.493737253992118319 ) ) ;
#5961 = ORIENTED_EDGE ( 'NONE', *, *, #2646, .T. ) ;
#5962 = ORIENTED_EDGE ( 'NONE', *, *, #7591, .F. ) ;
#5963 = ORIENTED_EDGE ( 'NONE', *, *, #3487, .T. ) ;
#5964 = ORIENTED_EDGE ( 'NONE', *, *, #2716, .F. ) ;
#5965 = CARTESIAN_POINT ( 'NONE',  ( -14.14213562373094568, -14.99999999999998757, -20.00000000000000000 ) ) ;
#5966 = DIRECTION ( 'NONE',  ( 0.000000000000000000, 1.000000000000000000, 0.000000000000000000 ) ) ;
#5967 = LINE ( 'NONE', #13332, #8881 ) ;
#5968 = DIRECTION ( 'NONE',  ( 0.000000000000000000, 0.000000000000000000, 1.000000000000000000 ) ) ;
#5969 =( GEOMETRIC_REPRESENTATION_CONTEXT ( 3 ) GLOBAL_UNCERTAINTY_ASSIGNED_CONTEXT ( ( #6265 ) ) GLOBAL_UNIT_ASSIGNED_CONTEXT ( ( #11082, #10042, #11151 ) ) REPRESENTATION_CONTEXT ( 'NONE', 'WORKASPACE' ) );
#5970 = EDGE_CURVE ( 'NONE', #11894, #12887, #7515, .T. ) ;
#5971 = AXIS2_PLACEMENT_3D ( 'NONE', #801, #7464, #5193 ) ;
#5972 = CARTESIAN_POINT ( 'NONE',  ( 44.91013252490152752, 62.79948385550240175, 3.727524721679198461 ) ) ;
#5973 = CARTESIAN_POINT ( 'NONE',  ( 55.96859303347802239, 50.80051614449766362, -4.306917132069484566 ) ) ;
#5974 = CARTESIAN_POINT ( 'NONE',  ( 42.39856655714564226, 58.10051614449765367, -2.493737253992044156 ) ) ;
#5975=STYLED_ITEM('',(#13691),#961);
#5976 = FACE_OUTER_BOUND ( 'NONE', #3535, .T. ) ;
#5977 = LINE ( 'NONE', #548, #5593 ) ;
#5978 = CARTESIAN_POINT ( 'NONE',  ( 49.97728705011495265, 47.50051614449765935, 8.000000000000001776 ) ) ;
#5980 = ORIENTED_EDGE ( 'NONE', *, *, #4324, .T. ) ;
#5979 = ORIENTED_EDGE ( 'NONE', *, *, #1344, .T. ) ;
#5981 = CARTESIAN_POINT ( 'NONE',  ( 32.49999999999998579, 40.00000000000001421, 5.000000000000002665 ) ) ;
#5982 = EDGE_LOOP ( 'NONE', ( #2694, #13577, #4319, #3735, #7270 ) ) ;
#5983 = ORIENTED_EDGE ( 'NONE', *, *, #5940, .F. ) ;
#5984 = DIRECTION ( 'NONE',  ( 0.000000000000000000, 0.000000000000000000, 1.000000000000000000 ) ) ;
#5985 = CARTESIAN_POINT ( 'NONE',  ( 53.50000000000000000, 0.000000000000000000, 0.000000000000000000 ) ) ;
#5986 = CONTEXT_DEPENDENT_SHAPE_REPRESENTATION ( #7608, #13056 ) ;
#5987 = CARTESIAN_POINT ( 'NONE',  ( 45.90387839640214196, 60.69948385550240033, 5.676469297603166098 ) ) ;
#5988 = CARTESIAN_POINT ( 'NONE',  ( 56.66441430157296821, 62.09948385550239891, 2.141517661632100111 ) ) ;
#5989 = VECTOR ( 'NONE', #3523, 1000.000000000000000 ) ;
#5990 = DIRECTION ( 'NONE',  ( -1.000000000000000000, 0.000000000000000000, 1.224646799147353207E-16 ) ) ;
#5991 = CARTESIAN_POINT ( 'NONE',  ( 2.449293598294706513E-15, -20.00000000000000000, 9.000000000000000000 ) ) ;
#5992 = PLANE ( 'NONE',  #1733 ) ;
#5993 = CARTESIAN_POINT ( 'NONE',  ( 47.70284917648459100, 45.60051614449765367, 6.992620115222796251 ) ) ;
#5994 = CARTESIAN_POINT ( 'NONE',  ( 44.91013252490152752, 52.79948385550240175, 3.727524721679198461 ) ) ;
#5995 = DIRECTION ( 'NONE',  ( -1.000000000000000000, -0.000000000000000000, -0.000000000000000000 ) ) ;
#5996 = EDGE_LOOP ( 'NONE', ( #616, #2082, #11442, #2715, #2769 ) ) ;
#5997 = EDGE_LOOP ( 'NONE', ( #4676, #7269, #363, #8275 ) ) ;
#5998 = VERTEX_POINT ( 'NONE', #9393 ) ;
#5999 = CARTESIAN_POINT ( 'NONE',  ( 4.000000000000000000, 2.309401076758497151, -3.433295621305379353 ) ) ;
#6000 = AXIS2_PLACEMENT_3D ( 'NONE', #3980, #2949, #4128 ) ;
#6001 = DIRECTION ( 'NONE',  ( -1.000000000000000000, 0.000000000000000000, -0.000000000000000000 ) ) ;
#6002 = CARTESIAN_POINT ( 'NONE',  ( 6.481779955677443361, -2.910222513313286186, 5.040653254389420468 ) ) ;
#6003 =( LENGTH_UNIT ( ) NAMED_UNIT ( * ) SI_UNIT ( .MILLI., .METRE. ) );
#6004 = CARTESIAN_POINT ( 'NONE',  ( 75.00000000000001421, 5.000000000000025757, 0.000000000000000000 ) ) ;
#6005 = DIRECTION ( 'NONE',  ( 0.9914448613738102711, -0.1305261922200524338, 0.000000000000000000 ) ) ;
#6006 = CARTESIAN_POINT ( 'NONE',  ( 44.91013252490152752, 64.79948385550240175, 3.727524721679198461 ) ) ;
#6007 = LINE ( 'NONE', #9111, #11599 ) ;
#6008 = CARTESIAN_POINT ( 'NONE',  ( 44.05948171654949874, 56.79948385550240886, 4.345558710429105354 ) ) ;
#6009 = CARTESIAN_POINT ( 'NONE',  ( 44.05948171654949874, 52.79948385550240175, 4.345558710429105354 ) ) ;
#6010 = AXIS2_PLACEMENT_3D ( 'NONE', #11238, #1758, #10275 ) ;
#6011 = VECTOR ( 'NONE', #5401, 1000.000000000000000 ) ;
#6012 = ORIENTED_EDGE ( 'NONE', *, *, #12241, .F. ) ;
#6013 = CARTESIAN_POINT ( 'NONE',  ( 45.90387839640214196, 46.69948385550240744, 5.676469297603166098 ) ) ;
#6014 = ORIENTED_EDGE ( 'NONE', *, *, #7461, .F. ) ;
#6015 = ORIENTED_EDGE ( 'NONE', *, *, #7381, .T. ) ;
#6016 = CARTESIAN_POINT ( 'NONE',  ( -7.500000000000013323, -7.009618943233427935, -9.000000000000000000 ) ) ;
#6017 = ORIENTED_EDGE ( 'NONE', *, *, #5773, .T. ) ;
#6018 = EDGE_CURVE ( 'NONE', #4606, #10246, #12052, .T. ) ;
#6019 = CARTESIAN_POINT ( 'NONE',  ( -2.000000000000002665, -3.464101615137770374, -3.142992957459237680 ) ) ;
#6020 = AXIS2_PLACEMENT_3D ( 'NONE', #12534, #3269, #903 ) ;
#6021 = B_SPLINE_CURVE_WITH_KNOTS ( 'NONE', 3,
 ( #12727, #2283, #3335, #7297 ),
 .UNSPECIFIED., .F., .F.,
 ( 4, 4 ),
 ( 0.002080789711329271950, 0.004173039763574510827 ),
 .UNSPECIFIED. ) ;
#6022 = LINE ( 'NONE', #800, #9160 ) ;
#6023 = AXIS2_PLACEMENT_3D ( 'NONE', #8942, #11982, #8800 ) ;
#6024 = AXIS2_PLACEMENT_3D ( 'NONE', #4818, #13232, #3777 ) ;
#6025 = CARTESIAN_POINT ( 'NONE',  ( 6.403457969954082785, -2.888443235695457467, -5.002930439003169916 ) ) ;
#6026 = CARTESIAN_POINT ( 'NONE',  ( 49.97728705011494554, 59.50051614449765935, 6.000000000000000888 ) ) ;
#6027 = FACE_OUTER_BOUND ( 'NONE', #67, .T. ) ;
#6028 = CARTESIAN_POINT ( 'NONE',  ( 56.81924384183011512, 56.19948385550240744, 4.924951120819313743 ) ) ;
#6029 = CARTESIAN_POINT ( 'NONE',  ( 57.36023556966787851, 61.99948385550241170, -0.02388180880522424582 ) ) ;
#6030 = CARTESIAN_POINT ( 'NONE',  ( 62.49999999999998579, 45.00000000000001421, 9.999999999999998224 ) ) ;
#6031 = EDGE_CURVE ( 'NONE', #3891, #6039, #5294, .T. ) ;
#6032 = ADVANCED_FACE ( 'NONE', ( #5577 ), #3359, .F. ) ;
#6033 = CARTESIAN_POINT ( 'NONE',  ( 49.97728705011486738, 47.49948385550240459, -8.000000000000001776 ) ) ;
#6034 = EDGE_CURVE ( 'NONE', #2414, #1065, #3562, .T. ) ;
#6035 = VERTEX_POINT ( 'NONE', #8820 ) ;
#6036 = ORIENTED_EDGE ( 'NONE', *, *, #7625, .T. ) ;
#6037 = VECTOR ( 'NONE', #8741, 1000.000000000000000 ) ;
#6038 = ADVANCED_FACE ( 'NONE', ( #174 ), #2377, .T. ) ;
#6039 = VERTEX_POINT ( 'NONE', #11923 ) ;
#6040 = CARTESIAN_POINT ( 'NONE',  ( -4.211140560182196957, -2.431303136016552013, -3.745885042887436178 ) ) ;
#6041 = CARTESIAN_POINT ( 'NONE',  ( 62.49999999999998579, 40.00000000000001421, 0.000000000000000000 ) ) ;
#6042 = DIRECTION ( 'NONE',  ( 0.000000000000000000, 0.000000000000000000, -1.000000000000000000 ) ) ;
#6043 = CARTESIAN_POINT ( 'NONE',  ( 2.000000000000000000, -0.8865213383406694847, 1.535500000000001419 ) ) ;
#6044 = CARTESIAN_POINT ( 'NONE',  ( 0.3108895250735811966, -2.416698868092462149, 4.999999999999999112 ) ) ;
#6045 = CARTESIAN_POINT ( 'NONE',  ( 53.50833635130540955, 63.69948385550240033, -4.867452303228209765 ) ) ;
#6046 = CARTESIAN_POINT ( 'NONE',  ( 56.65037692655921120, 51.10051614449766078, 2.184720259617097593 ) ) ;
#6047 = CARTESIAN_POINT ( 'NONE',  ( 54.72065718078918906, 58.70051614449765509, -6.458785618021089192 ) ) ;
#6048 = AXIS2_PLACEMENT_3D ( 'NONE', #2551, #9880, #9948 ) ;
#6049 = CARTESIAN_POINT ( 'NONE',  ( 4.000000000000000000, 0.000000000000000000, 0.000000000000000000 ) ) ;
#6050 = CARTESIAN_POINT ( 'NONE',  ( 54.68390685589039890, 51.30051614449765651, 6.485486291978072693 ) ) ;
#6052 = ORIENTED_EDGE ( 'NONE', *, *, #8193, .T. ) ;
#6051 = VERTEX_POINT ( 'NONE', #371 ) ;
#6053 = CLOSED_SHELL ( 'NONE', ( #12944, #13604, #11518, #5639, #7976, #4089, #12854, #7212, #2924, #1640, #707, #5850, #2019, #11161, #12167, #6159, #12440, #11615, #10670, #5256, #3973, #454, #3571, #7141, #7631, #10793, #10514, #3316, #6456 ) ) ;
#6054 = AXIS2_PLACEMENT_3D ( 'NONE', #2813, #6399, #1106 ) ;
#6055 = ORIENTED_EDGE ( 'NONE', *, *, #883, .F. ) ;
#6056 = EDGE_CURVE ( 'NONE', #7551, #5348, #5135, .T. ) ;
#6057 = EDGE_LOOP ( 'NONE', ( #8168, #1400 ) ) ;
#6058 = ORIENTED_EDGE ( 'NONE', *, *, #706, .F. ) ;
#6059 = CARTESIAN_POINT ( 'NONE',  ( 2.449293598294706513E-15, -20.00000000000000000, -23.00000000000000000 ) ) ;
#6060 = CARTESIAN_POINT ( 'NONE',  ( 2.449293598294706513E-15, -35.00000000000000000, -9.000000000000000000 ) ) ;
#6061 = PRODUCT_CONTEXT ( 'NONE', #10163, 'mechanical' ) ;
#6062 = CARTESIAN_POINT ( 'NONE',  ( 48.07319477248768180, 46.59948385550239891, 6.007379884777225953 ) ) ;
#6063 = CARTESIAN_POINT ( 'NONE',  ( 54.13287192849676188, 56.29948385550240175, 5.649768623646098220 ) ) ;
#6064 = DIRECTION ( 'NONE',  ( -1.000000000000000000, -0.000000000000000000, -0.000000000000000000 ) ) ;
#6065 = DIRECTION ( 'NONE',  ( 0.6040472319084893016, -0.7969485188038759604, -1.107688701425240097E-17 ) ) ;
#6066 = DIRECTION ( 'NONE',  ( 0.000000000000000000, 0.000000000000000000, 1.000000000000000000 ) ) ;
#6067 = CARTESIAN_POINT ( 'NONE',  ( 52.25172492374527877, 53.40051614449765793, 7.007379884777203749 ) ) ;
#6068 = CARTESIAN_POINT ( 'NONE',  ( 50.02271294988511841, 54.49948385550240459, 6.000000000000000888 ) ) ;
#6069 = CARTESIAN_POINT ( 'NONE',  ( 2.449293598294706513E-15, -20.00000000000000000, 9.000000000000000000 ) ) ;
#6070 = VECTOR ( 'NONE', #7025, 1000.000000000000000 ) ;
#6071 = EDGE_LOOP ( 'NONE', ( #6935, #5685 ) ) ;
#6072 = EDGE_CURVE ( 'NONE', #12234, #3300, #9914, .T. ) ;
#6073 = EDGE_CURVE ( 'NONE', #8324, #8131, #8920, .T. ) ;
#6074 = ORIENTED_EDGE ( 'NONE', *, *, #1946, .T. ) ;
#6075 = ORIENTED_EDGE ( 'NONE', *, *, #13206, .T. ) ;
#6076 = CARTESIAN_POINT ( 'NONE',  ( 4.175813232069148562, -2.061359961916374051, -3.570380186727397653 ) ) ;
#6077 = CARTESIAN_POINT ( 'NONE',  ( 6.507056315241514177, 2.833450876375910976, -5.092319121366348789 ) ) ;
#6078 = FACE_OUTER_BOUND ( 'NONE', #4301, .T. ) ;
#6079 = FILL_AREA_STYLE_COLOUR ( '', #4187 ) ;
#6080 = CARTESIAN_POINT ( 'NONE',  ( 56.65037692655918988, 45.89948385550240317, -2.184720259617163762 ) ) ;
#6081 = SURFACE_STYLE_USAGE ( .BOTH. , #1833 ) ;
#6082 = AXIS2_PLACEMENT_3D ( 'NONE', #2149, #8526, #9491 ) ;
#6083 = CARTESIAN_POINT ( 'NONE',  ( 6.207519134555854023, 1.039264565631282888, -4.999999999999109157 ) ) ;
#6084 = CARTESIAN_POINT ( 'NONE',  ( 46.49166364869460466, 64.69948385550240744, 4.867452303228209765 ) ) ;
#6085 = CARTESIAN_POINT ( 'NONE',  ( 14.92500000000001492, -21.49812382665770727, 9.000000000000000000 ) ) ;
#6086 = AXIS2_PLACEMENT_3D ( 'NONE', #7237, #8408, #9303 ) ;
#6087 = CARTESIAN_POINT ( 'NONE',  ( 44.05948171654949874, 58.79948385550240886, 4.345558710429105354 ) ) ;
#6088 = CARTESIAN_POINT ( 'NONE',  ( 45.90387839640214196, 54.69948385550240744, 5.676469297603166098 ) ) ;
#6089 = VECTOR ( 'NONE', #1992, 1000.000000000000000 ) ;
#6090 = ORIENTED_EDGE ( 'NONE', *, *, #6601, .F. ) ;
#6091 = CARTESIAN_POINT ( 'NONE',  ( 55.96859303347804371, 52.19948385550240033, 4.306917132069425946 ) ) ;
#6092 = AXIS2_PLACEMENT_3D ( 'NONE', #265, #5472, #9675 ) ;
#6093 = ORIENTED_EDGE ( 'NONE', *, *, #1863, .F. ) ;
#6094 = CARTESIAN_POINT ( 'NONE',  ( -2.595115354961444076, -7.673029147243174641, -1.000000000000000000 ) ) ;
#6095 = VERTEX_POINT ( 'NONE', #4533 ) ;
#6096 = DIRECTION ( 'NONE',  ( 0.000000000000000000, 0.000000000000000000, -1.000000000000000000 ) ) ;
#6097 = CARTESIAN_POINT ( 'NONE',  ( 4.799999999999999822, 0.000000000000000000, 0.000000000000000000 ) ) ;
#6098 = ADVANCED_FACE ( 'NONE', ( #11998 ), #10881, .T. ) ;
#6099 = CARTESIAN_POINT ( 'NONE',  ( 47.70284917648453415, 49.39948385550239607, -6.992620115222774047 ) ) ;
#6100 = CARTESIAN_POINT ( 'NONE',  ( 55.69932041026405045, 63.10051614449766078, 1.875703265242156359 ) ) ;
#6101 = CARTESIAN_POINT ( 'NONE',  ( 75.00000000000000000, 40.00000000000000000, -10.00000000000000000 ) ) ;
#6102 = CARTESIAN_POINT ( 'NONE',  ( 56.79116909180255135, 57.79948385550240175, -4.963592699179005585 ) ) ;
#6103 = CARTESIAN_POINT ( 'NONE',  ( 44.03140696652192787, 63.19948385550240744, -4.306917132069425058 ) ) ;
#6104 = CARTESIAN_POINT ( 'NONE',  ( 20.00000000000000000, -25.00000000000000711, -20.00000000000000000 ) ) ;
#6105 = CARTESIAN_POINT ( 'NONE',  ( 57.61547081786812896, 48.09948385550240602, 2.450534656007040901 ) ) ;
#6106 = ORIENTED_EDGE ( 'NONE', *, *, #5013, .F. ) ;
#6107 = VERTEX_POINT ( 'NONE', #4392 ) ;
#6108 = ORIENTED_EDGE ( 'NONE', *, *, #4324, .F. ) ;
#6109 = CARTESIAN_POINT ( 'NONE',  ( 30.00000000000000355, -39.99999999999998579, -10.00000000000000178 ) ) ;
#6110 = SURFACE_STYLE_FILL_AREA ( #2699 ) ;
#6111 = CARTESIAN_POINT ( 'NONE',  ( 62.49999999999998579, 5.000000000000018652, 5.000000000000000000 ) ) ;
#6112 = PLANE ( 'NONE',  #8852 ) ;
#6113 = CARTESIAN_POINT ( 'NONE',  ( 13.61000000000001009, 0.000000000000000000, 0.000000000000000000 ) ) ;
#6114 = CARTESIAN_POINT ( 'NONE',  ( 44.30067958973596376, 64.89948385550239607, 1.875703265242204099 ) ) ;
#6115 = CARTESIAN_POINT ( 'NONE',  ( 42.63976443033212149, 52.00051614449765935, -0.02388180880514948964 ) ) ;
#6116 = CARTESIAN_POINT ( 'NONE',  ( 52.62207051974829852, 56.60051614449765367, -7.992620115222797139 ) ) ;
#6117 = DIRECTION ( 'NONE',  ( 0.8660254037844381525, 0.5000000000000009992, 0.000000000000000000 ) ) ;
#6118 = CARTESIAN_POINT ( 'NONE',  ( 42.38452918213190657, 51.90051614449765793, 2.450534656007115508 ) ) ;
#6119 = AXIS2_PLACEMENT_3D ( 'NONE', #5991, #3632, #625 ) ;
#6121 = EDGE_LOOP ( 'NONE', ( #5905, #7222, #12939, #2347 ) ) ;
#6120 = VERTEX_POINT ( 'NONE', #5511 ) ;
#6122 = ORIENTED_EDGE ( 'NONE', *, *, #6453, .F. ) ;
#6123 = PRODUCT_DEFINITION_CONTEXT ( 'detailed design', #10613, 'design' ) ;
#6124 = ORIENTED_EDGE ( 'NONE', *, *, #1650, .F. ) ;
#6125 = DIRECTION ( 'NONE',  ( -1.000000000000000000, 0.000000000000000000, -0.000000000000000000 ) ) ;
#6126 = DIRECTION ( 'NONE',  ( -1.000000000000000000, 0.000000000000000000, -0.000000000000000000 ) ) ;
#6127 = DIRECTION ( 'NONE',  ( 0.000000000000000000, 0.000000000000000000, 1.000000000000000000 ) ) ;
#6128 = APPLICATION_CONTEXT ( 'automotive_design' ) ;
#6129 = PRODUCT_CONTEXT ( 'NONE', #5673, 'mechanical' ) ;
#6130 = CARTESIAN_POINT ( 'NONE',  ( 55.96859303347804371, 62.19948385550240744, 4.306917132069425946 ) ) ;
#6131 = CARTESIAN_POINT ( 'NONE',  ( 43.33558569842703179, 59.09948385550240602, -2.141517661632099223 ) ) ;
#6132 = EDGE_CURVE ( 'NONE', #3385, #9486, #7496, .T. ) ;
#6133 = EDGE_CURVE ( 'NONE', #11305, #9887, #4462, .T. ) ;
#6134 = DIRECTION ( 'NONE',  ( 0.000000000000000000, 1.000000000000000000, 0.000000000000000000 ) ) ;
#6135 = DIRECTION ( 'NONE',  ( -0.8571673013836855759, 0.000000000000000000, -0.5150380737757258576 ) ) ;
#6136 = CARTESIAN_POINT ( 'NONE',  ( 54.56344682779376143, 44.99999999999996447, -5.899875555194201482 ) ) ;
#6137 = CARTESIAN_POINT ( 'NONE',  ( 45.86712807150329496, 49.70051614449766220, 5.649768623646139964 ) ) ;
#6138 = CARTESIAN_POINT ( 'NONE',  ( 46.49166364869460466, 52.69948385550240744, 4.867452303228209765 ) ) ;
#6139 = CARTESIAN_POINT ( 'NONE',  ( 8.759913291900311094, -7.823632761846075923, -9.000000000000000000 ) ) ;
#6140 = EDGE_CURVE ( 'NONE', #1099, #6957, #3429, .T. ) ;
#6141 = ORIENTED_EDGE ( 'NONE', *, *, #8531, .F. ) ;
#6142 = LINE ( 'NONE', #8411, #2626 ) ;
#6143 = ORIENTED_EDGE ( 'NONE', *, *, #13179, .T. ) ;
#6144 = VERTEX_POINT ( 'NONE', #11857 ) ;
#6145 = DIRECTION ( 'NONE',  ( 0.000000000000000000, 0.000000000000000000, 1.000000000000000000 ) ) ;
#6146 = CARTESIAN_POINT ( 'NONE',  ( 1.000000000000000444, -15.10102051443364246, 15.00000000000000355 ) ) ;
#6147 = CARTESIAN_POINT ( 'NONE',  ( 6.466260427357672036, -2.904280683598005286, 5.030361703432631337 ) ) ;
#6148 = B_SPLINE_CURVE_WITH_KNOTS ( 'NONE', 3,
 ( #9002, #11207, #5902, #8303, #12184, #10177 ),
 .UNSPECIFIED., .F., .F.,
 ( 4, 2, 4 ),
 ( 0.005852013098461904955, 0.006875955139453157790, 0.007899897180444410624 ),
 .UNSPECIFIED. ) ;
#6149 = DIRECTION ( 'NONE',  ( 1.000000000000000000, 0.000000000000000000, 0.000000000000000000 ) ) ;
#6150 = CARTESIAN_POINT ( 'NONE',  ( -1.257172072275743346, 3.892973519171203378, -3.433252694550776862 ) ) ;
#6151 = CARTESIAN_POINT ( 'NONE',  ( 48.07319477248762496, 46.40051614449765793, -6.007379884777208190 ) ) ;
#6152 = DIRECTION ( 'NONE',  ( -0.000000000000000000, -0.000000000000000000, 1.000000000000000000 ) ) ;
#6153 = CARTESIAN_POINT ( 'NONE',  ( 55.94051828345050836, 55.79948385550238044, -4.345558710429104465 ) ) ;
#6154 = CARTESIAN_POINT ( 'NONE',  ( 55.94051828345050836, 55.79948385550238044, -4.345558710429104465 ) ) ;
#6155 = VERTEX_POINT ( 'NONE', #1330 ) ;
#6156 = CARTESIAN_POINT ( 'NONE',  ( 49.97728705011488159, 47.49948385550240459, -7.000000000000000888 ) ) ;
#6157 = ORIENTED_EDGE ( 'NONE', *, *, #9007, .F. ) ;
#6158 = DIRECTION ( 'NONE',  ( 1.000000000000000000, -1.734723475976807341E-16, 0.000000000000000000 ) ) ;
#6159 = ADVANCED_FACE ( 'NONE', ( #5647 ), #8813, .T. ) ;
#6160 = ORIENTED_EDGE ( 'NONE', *, *, #1775, .F. ) ;
#6161 = DIRECTION ( 'NONE',  ( -0.000000000000000000, -0.000000000000000000, 1.000000000000000000 ) ) ;
#6162 = DIRECTION ( 'NONE',  ( -1.000000000000000000, -0.000000000000000000, -0.000000000000000000 ) ) ;
#6163 = CARTESIAN_POINT ( 'NONE',  ( 54.13287192849676188, 46.29948385550240886, 5.649768623646098220 ) ) ;
#6164 = CARTESIAN_POINT ( 'NONE',  ( 47.74827507625469281, 48.40051614449764372, -7.007379884777203749 ) ) ;
#6165 = CARTESIAN_POINT ( 'NONE',  ( -4.000000000000000888, 1.563622288139195238, -0.2253451193528307472 ) ) ;
#6166 = ADVANCED_FACE ( 'NONE', ( #6748 ), #1467, .F. ) ;
#6167 = CARTESIAN_POINT ( 'NONE',  ( 56.81924384183011512, 60.19948385550240744, 4.924951120819313743 ) ) ;
#6168 = CARTESIAN_POINT ( 'NONE',  ( -9.999999999999996447, 25.00000000000001776, 15.00000000000000000 ) ) ;
#6169 = CARTESIAN_POINT ( 'NONE',  ( 43.18075615816989199, 47.19948385550240744, -4.924951120819313743 ) ) ;
#6170 = ORIENTED_EDGE ( 'NONE', *, *, #5151, .F. ) ;
#6171 = EDGE_LOOP ( 'NONE', ( #6540, #4520, #10921, #12851 ) ) ;
#6172 = ORIENTED_EDGE ( 'NONE', *, *, #9481, .T. ) ;
#6173 = VECTOR ( 'NONE', #1474, 1000.000000000000000 ) ;
#6174 = ADVANCED_FACE ( 'NONE', ( #8955 ), #3901, .F. ) ;
#6175 = DIRECTION ( 'NONE',  ( 1.000000000000000000, 0.000000000000000000, 0.000000000000000000 ) ) ;
#6176 = VECTOR ( 'NONE', #6290, 1000.000000000000000 ) ;
#6177 = PRODUCT_RELATED_PRODUCT_CATEGORY ( 'part', '', ( #443 ) ) ;
#6178 =( LENGTH_UNIT ( ) NAMED_UNIT ( * ) SI_UNIT ( .MILLI., .METRE. ) );
#6179 = FACE_OUTER_BOUND ( 'NONE', #1881, .T. ) ;
#6180 = LINE ( 'NONE', #3186, #9944 ) ;
#6181 = DIRECTION ( 'NONE',  ( 0.000000000000000000, 0.000000000000000000, 1.000000000000000000 ) ) ;
#6182 = CARTESIAN_POINT ( 'NONE',  ( 53.54508667620424234, 44.70051614449765509, -4.840751629271188961 ) ) ;
#6183 = CARTESIAN_POINT ( 'NONE',  ( 55.94051828345054389, 51.20051614449765509, 4.345558710429044957 ) ) ;
#6184 = CARTESIAN_POINT ( 'NONE',  ( 50.02271294988505446, 60.50051614449766646, -8.000000000000001776 ) ) ;
#6185 = AXIS2_PLACEMENT_3D ( 'NONE', #8808, #11988, #4592 ) ;
#6186 = CARTESIAN_POINT ( 'NONE',  ( 62.49999999999998579, 45.00000000000001421, 15.00000000000000000 ) ) ;
#6187 = CARTESIAN_POINT ( 'NONE',  ( 56.79116909180259398, 51.20051614449766220, 4.963592699178938972 ) ) ;
#6189 = ORIENTED_EDGE ( 'NONE', *, *, #12099, .F. ) ;
#6188 = ORIENTED_EDGE ( 'NONE', *, *, #10320, .T. ) ;
#6190 = ORIENTED_EDGE ( 'NONE', *, *, #9145, .T. ) ;
#6191 = ORIENTED_EDGE ( 'NONE', *, *, #2727, .T. ) ;
#6192 = DIRECTION ( 'NONE',  ( -0.000000000000000000, 0.000000000000000000, -1.000000000000000000 ) ) ;
#6194 = VECTOR ( 'NONE', #13119, 999.9999999999998863 ) ;
#6193 = CARTESIAN_POINT ( 'NONE',  ( 6.534533895392294234, 2.951347675328729991, -5.111884124469655788 ) ) ;
#6195 = CARTESIAN_POINT ( 'NONE',  ( -3.417495597855351487E-15, 4.207632145829744097, -2.712167343862822655 ) ) ;
#6196 = DIRECTION ( 'NONE',  ( -1.000000000000000000, 0.000000000000000000, 0.000000000000000000 ) ) ;
#6197 = APPLICATION_PROTOCOL_DEFINITION ( 'draft international standard', 'automotive_design', 1998, #1148 ) ;
#6198 = CARTESIAN_POINT ( 'NONE',  ( 50.02271294988512551, 62.49948385550240459, 7.000000000000000888 ) ) ;
#6199 = CARTESIAN_POINT ( 'NONE',  ( 56.65037692655918988, 57.89948385550240317, -2.184720259617163762 ) ) ;
#6200 = ADVANCED_FACE ( 'NONE', ( #13426 ), #5024, .F. ) ;
#6201 = CARTESIAN_POINT ( 'NONE',  ( 50.02271294988505446, 60.50051614449765935, -7.000000000000000888 ) ) ;
#6202 = DIRECTION ( 'NONE',  ( 0.000000000000000000, -0.5000000000000011102, -0.8660254037844379305 ) ) ;
#6203 = DIRECTION ( 'NONE',  ( -0.000000000000000000, -0.000000000000000000, -1.000000000000000000 ) ) ;
#6204 = AXIS2_PLACEMENT_3D ( 'NONE', #5642, #5911, #4734 ) ;
#6205 = CARTESIAN_POINT ( 'NONE',  ( 4.630153689607048761, 0.000000000000000000, -5.371010071662833063 ) ) ;
#6206 = CARTESIAN_POINT ( 'NONE',  ( 47.74827507625469281, 52.40051614449763662, -7.007379884777203749 ) ) ;
#6207 = CARTESIAN_POINT ( 'NONE',  ( 43.69122665457040000, 54.99948385550239749, 0.02388180880521036456 ) ) ;
#6208 = VECTOR ( 'NONE', #7178, 1000.000000000000000 ) ;
#6209 = LINE ( 'NONE', #10608, #963 ) ;
#6210 = EDGE_CURVE ( 'NONE', #10817, #4979, #3954, .T. ) ;
#6211 = ORIENTED_EDGE ( 'NONE', *, *, #1902, .F. ) ;
#6212 = CARTESIAN_POINT ( 'NONE',  ( 4.000000000000000000, 2.309401076758497151, -5.000000000000000000 ) ) ;
#6213 = ADVANCED_FACE ( 'NONE', ( #1603 ), #10576, .F. ) ;
#6214 = ORIENTED_EDGE ( 'NONE', *, *, #1611, .F. ) ;
#6216 = ADVANCED_FACE ( 'NONE', ( #12130, #2726 ), #5992, .T. ) ;
#6215 = ORIENTED_EDGE ( 'NONE', *, *, #10570, .F. ) ;
#6217 = DIRECTION ( 'NONE',  ( 1.000000000000000000, 0.000000000000000000, 0.000000000000000000 ) ) ;
#6218 =( REPRESENTATION_RELATIONSHIP ('NONE','NONE', #5328, #180 ) REPRESENTATION_RELATIONSHIP_WITH_TRANSFORMATION ( #4641 )SHAPE_REPRESENTATION_RELATIONSHIP( ) );
#6219 = EDGE_CURVE ( 'NONE', #8131, #6586, #8264, .T. ) ;
#6220 = CARTESIAN_POINT ( 'NONE',  ( 6.541171661047875396, 5.920857802016174176, 0.02973393389964464062 ) ) ;
#6221 = CARTESIAN_POINT ( 'NONE',  ( 6.533910050139693837, -2.950514251728023840, 5.110440592449081443 ) ) ;
#6222 = SHAPE_REPRESENTATION_RELATIONSHIP ( 'NONE' , 'NONE' ,  #5848, #7343 ) ;
#6223 = CARTESIAN_POINT ( 'NONE',  ( 55.96859303347804371, 46.19948385550238612, 4.306917132069425946 ) ) ;
#6224 = AXIS2_PLACEMENT_3D ( 'NONE', #8646, #10912, #1360 ) ;
#6225 = EDGE_CURVE ( 'NONE', #8791, #1824, #1066, .T. ) ;
#6226 = CARTESIAN_POINT ( 'NONE',  ( -20.00000000000000000, -19.99999999999999289, -12.00000000000000000 ) ) ;
#6227 = CARTESIAN_POINT ( 'NONE',  ( 44.30067958973596376, 64.89948385550239607, 1.875703265242204099 ) ) ;
#6228 = CARTESIAN_POINT ( 'NONE',  ( 56.66441430157296821, 64.09948385550239891, 2.141517661632100111 ) ) ;
#6229 = CARTESIAN_POINT ( 'NONE',  ( 50.02271294988512551, 54.49948385550240459, 7.000000000000000888 ) ) ;
#6230 = VERTEX_POINT ( 'NONE', #11157 ) ;
#6231 = CARTESIAN_POINT ( 'NONE',  ( 45.90387839640214196, 52.69948385550240033, 5.676469297603166098 ) ) ;
#6232 = B_SPLINE_CURVE_WITH_KNOTS ( 'NONE', 3,
 ( #7926, #7798, #7863, #2525, #4680, #8963 ),
 .UNSPECIFIED., .F., .F.,
 ( 4, 2, 4 ),
 ( 0.002452478801916361129, 0.003676905084148001344, 0.004901331366379641126 ),
 .UNSPECIFIED. ) ;
#6233 = AXIS2_PLACEMENT_3D ( 'NONE', #7050, #2900, #8161 ) ;
#6234 = ORIENTED_EDGE ( 'NONE', *, *, #5284, .F. ) ;
#6235 = LINE ( 'NONE', #6094, #1717 ) ;
#6236 = ORIENTED_EDGE ( 'NONE', *, *, #4226, .F. ) ;
#6237 = CARTESIAN_POINT ( 'NONE',  ( 4.093692494532771953, 2.021783646005768542, 3.501831996793843160 ) ) ;
#6238 = CARTESIAN_POINT ( 'NONE',  ( -30.00000000000000000, -1.040834085586084257E-14, 0.000000000000000000 ) ) ;
#6239 = CARTESIAN_POINT ( 'NONE',  ( 55.94051828345050836, 45.79948385550240886, -4.345558710429103577 ) ) ;
#6240 = AXIS2_PLACEMENT_3D ( 'NONE', #7781, #2371, #12123 ) ;
#6241 = CARTESIAN_POINT ( 'NONE',  ( 50.02271294988506156, 64.50051614449766646, -6.000000000000000888 ) ) ;
#6242 = CARTESIAN_POINT ( 'NONE',  ( 2.595115354961440524, -7.673029147243177306, 0.000000000000000000 ) ) ;
#6243 = CARTESIAN_POINT ( 'NONE',  ( 55.96859303347804371, 48.19948385550240033, 4.306917132069425946 ) ) ;
#6244 = PLANE ( 'NONE',  #6698 ) ;
#6245 = CARTESIAN_POINT ( 'NONE',  ( 54.68390685589033495, 49.69948385550240744, -6.485486291978119766 ) ) ;
#6246 = VERTEX_POINT ( 'NONE', #11087 ) ;
#6247 = CIRCLE ( 'NONE', #7108, 4.799999999999999822 ) ;
#6248 = ORIENTED_EDGE ( 'NONE', *, *, #7493, .F. ) ;
#6249 = ORIENTED_EDGE ( 'NONE', *, *, #1435, .F. ) ;
#6250 = EDGE_CURVE ( 'NONE', #10723, #4470, #4623, .T. ) ;
#6251 = VECTOR ( 'NONE', #2358, 1000.000000000000000 ) ;
#6252 = AXIS2_PLACEMENT_3D ( 'NONE', #12948, #2443, #11788 ) ;
#6253 = DIRECTION ( 'NONE',  ( 0.000000000000000000, -1.000000000000000000, 0.000000000000000000 ) ) ;
#6254 = DIRECTION ( 'NONE',  ( -1.000000000000000000, 0.000000000000000000, 0.000000000000000000 ) ) ;
#6255 = CARTESIAN_POINT ( 'NONE',  ( -74.99999999999997158, 20.00000000000001421, 15.00000000000000000 ) ) ;
#6256 = CARTESIAN_POINT ( 'NONE',  ( 1.000000000000000444, -15.10102051443364246, 9.000000000000000000 ) ) ;
#6257 = CARTESIAN_POINT ( 'NONE',  ( 46.45491332379576477, 45.70051614449766220, 4.840751629271188961 ) ) ;
#6258 = CARTESIAN_POINT ( 'NONE',  ( 56.66441430157294690, 58.90051614449766504, -2.141517661632166281 ) ) ;
#6259 = CARTESIAN_POINT ( 'NONE',  ( 54.68390685589039890, 61.30051614449766362, 6.485486291978072693 ) ) ;
#6260 = CONICAL_SURFACE ( 'NONE', #10862, 1.999999999999998224, 1.029744259999999745 ) ;
#6261 = CARTESIAN_POINT ( 'NONE',  ( -4.211405944401398038, -2.460460786169389902, -3.751298493805494072 ) ) ;
#6262 = CARTESIAN_POINT ( 'NONE',  ( 43.20883090819742023, 52.20051614449766220, -4.963592699178938972 ) ) ;
#6263 = ORIENTED_EDGE ( 'NONE', *, *, #2727, .F. ) ;
#6264 = VERTEX_POINT ( 'NONE', #1675 ) ;
#6265 = UNCERTAINTY_MEASURE_WITH_UNIT (LENGTH_MEASURE( 1.000000000000000082E-05 ), #11082, 'distance_accuracy_value', 'NONE');
#6266 = VERTEX_POINT ( 'NONE', #8126 ) ;
#6267 = CARTESIAN_POINT ( 'NONE',  ( 6.367873360227558344, 5.773502691896261751, 0.000000000000000000 ) ) ;
#6268 = DIRECTION ( 'NONE',  ( 1.000000000000000000, 0.000000000000000000, -0.000000000000000000 ) ) ;
#6269 = CARTESIAN_POINT ( 'NONE',  ( 0.1999999999999987899, 0.000000000000000000, 3.299999999999999822 ) ) ;
#6270 = CARTESIAN_POINT ( 'NONE',  ( 0.04320752586819883584, 0.9836842030436125928, -5.000000000000000000 ) ) ;
#6271 = CARTESIAN_POINT ( 'NONE',  ( 50.02271294988511841, 50.49948385550239749, 6.000000000000000888 ) ) ;
#6272 = CARTESIAN_POINT ( 'NONE',  ( 4.200000000000001954, 2.694222958124178486E-16, 2.200000000000001066 ) ) ;
#6273 = ADVANCED_FACE ( 'NONE', ( #10047 ), #562, .F. ) ;
#6274 = CARTESIAN_POINT ( 'NONE',  ( 57.36023556966787851, 61.00051614449766646, 0.02388180880515038476 ) ) ;
#6275 = AXIS2_PLACEMENT_3D ( 'NONE', #3401, #1442, #6588 ) ;
#6276 = CARTESIAN_POINT ( 'NONE',  ( -4.999999999999998224, -20.00000000000000000, -8.999999999999998224 ) ) ;
#6277 = CARTESIAN_POINT ( 'NONE',  ( -74.99999999999997158, 40.00000000000001421, 10.00000000000000000 ) ) ;
#6278 = LINE ( 'NONE', #4248, #8666 ) ;
#6279 = CARTESIAN_POINT ( 'NONE',  ( 44.03140696652198471, 49.80051614449766362, 4.306917132069485454 ) ) ;
#6280 = CARTESIAN_POINT ( 'NONE',  ( 55.11794222512601493, 58.19948385550240744, 3.688883143319541702 ) ) ;
#6281 = CARTESIAN_POINT ( 'NONE',  ( 55.11928596558036020, 44.77036257738321012, -5.000000000000000888 ) ) ;
#6282 = ADVANCED_FACE ( 'NONE', ( #13217 ), #1537, .T. ) ;
#6283 = ORIENTED_EDGE ( 'NONE', *, *, #10554, .F. ) ;
#6284 = DIRECTION ( 'NONE',  ( -9.858538378746663627E-23, 5.031452844637890958E-23, -1.000000000000000000 ) ) ;
#6285 = ORIENTED_EDGE ( 'NONE', *, *, #3039, .F. ) ;
#6286 = ORIENTED_EDGE ( 'NONE', *, *, #4754, .F. ) ;
#6287 = CARTESIAN_POINT ( 'NONE',  ( -12.17636723815382993, -11.24008670809956456, 0.000000000000000000 ) ) ;
#6288 = FACE_OUTER_BOUND ( 'NONE', #13410, .T. ) ;
#6289 = CARTESIAN_POINT ( 'NONE',  ( 4.071447262713887127, 2.020725942163686284, -3.499999999999999556 ) ) ;
#6290 = DIRECTION ( 'NONE',  ( -1.000000000000000000, -0.000000000000000000, -0.000000000000000000 ) ) ;
#6291 = EDGE_CURVE ( 'NONE', #486, #11340, #8596, .T. ) ;
#6292 = CARTESIAN_POINT ( 'NONE',  ( 51.92680522751238925, 51.40051614449767214, 6.007379884777208190 ) ) ;
#6293 = ADVANCED_FACE ( 'NONE', ( #5784 ), #13434, .T. ) ;
#6294 = CARTESIAN_POINT ( 'NONE',  ( 2.449293598294706513E-15, -20.00000000000000000, -9.000000000000000000 ) ) ;
#6295 = CARTESIAN_POINT ( 'NONE',  ( 47.70284917648453415, 65.39948385550239607, -6.992620115222774047 ) ) ;
#6296 = CARTESIAN_POINT ( 'NONE',  ( 44.03140696652192787, 61.19948385550239323, -4.306917132069425058 ) ) ;
#6297 = EDGE_CURVE ( 'NONE', #1406, #11112, #11227, .T. ) ;
#6298 = EDGE_LOOP ( 'NONE', ( #8861, #13282, #1771, #598 ) ) ;
#6299 = ORIENTED_EDGE ( 'NONE', *, *, #1511, .T. ) ;
#6300 = DIRECTION ( 'NONE',  ( -0.000000000000000000, -0.000000000000000000, 1.000000000000000000 ) ) ;
#6301 = CARTESIAN_POINT ( 'NONE',  ( 2.449293598294706513E-15, -20.00000000000000000, -20.00000000000000000 ) ) ;
#6302 = DIRECTION ( 'NONE',  ( -0.000000000000000000, -0.000000000000000000, 1.000000000000000000 ) ) ;
#6303 = CYLINDRICAL_SURFACE ( 'NONE', #2521, 5.000000000000007994 ) ;
#6304 = CARTESIAN_POINT ( 'NONE',  ( 30.00000000000000000, -7.499999999999991118, 10.00000000000000000 ) ) ;
#6305 = CIRCLE ( 'NONE', #11588, 15.00000000000000000 ) ;
#6306 = CARTESIAN_POINT ( 'NONE',  ( 43.34962307344078880, 50.10051614449766078, -2.184720259617096705 ) ) ;
#6307 = CARTESIAN_POINT ( 'NONE',  ( -4.000000000000000000, 0.1981133338132459731, 2.096406544454392723E-17 ) ) ;
#6308 = AXIS2_PLACEMENT_3D ( 'NONE', #11682, #10649, #1163 ) ;
#6309 =( BOUNDED_SURFACE ( )  B_SPLINE_SURFACE ( 3, 2, ( 
 ( #13579, #8349, #6220 ),
 ( #8207, #12553, #5175 ),
 ( #7316, #8069, #9103 ),
 ( #2809, #3017, #9381 ),
 ( #3911, #9242, #7172 ),
 ( #1829, #6077, #13505 ) ),
 .UNSPECIFIED., .F., .F., .F. ) 
 B_SPLINE_SURFACE_WITH_KNOTS ( ( 4, 2, 4 ),
 ( 3, 3 ),
 ( 0.02367865728600889938, 0.02663179453327095547, 0.02958493178053301503 ),
 ( 0.000000000000000000, 1.000000000000000000 ),
 .UNSPECIFIED. ) 
 GEOMETRIC_REPRESENTATION_ITEM ( )  RATIONAL_B_SPLINE_SURFACE ( (
 ( 1.000000000000000000, 0.8047781103519390244, 1.000000000000000000),
 ( 1.000000000000000000, 0.8123785825980075481, 1.000000000000000000),
 ( 1.000000000000000000, 0.8190671539288042480, 1.000000000000000000),
 ( 1.000000000000000000, 0.8192352255335092481, 1.000000000000000000),
 ( 1.000000000000000000, 0.8126129676835915916, 1.000000000000000000),
 ( 1.000000000000000000, 0.8047712537969718971, 1.000000000000000000) ) ) 
 REPRESENTATION_ITEM ( '' )  SURFACE ( )  );
#6310 = CARTESIAN_POINT ( 'NONE',  ( 56.79116909180255135, 63.79948385550241596, -4.963592699179005585 ) ) ;
#6311 = CARTESIAN_POINT ( 'NONE',  ( 50.02271294988505446, 44.50051614449765935, -7.000000000000000888 ) ) ;
#6312 = CIRCLE ( 'NONE', #5422, 1.499999999999999778 ) ;
#6313 = CARTESIAN_POINT ( 'NONE',  ( 58.41169779390614281, 57.99948385550241170, -0.02388180880523160798 ) ) ;
#6314 = ORIENTED_EDGE ( 'NONE', *, *, #3153, .F. ) ;
#6315 = AXIS2_PLACEMENT_3D ( 'NONE', #6294, #9449, #2175 ) ;
#6316 = ORIENTED_EDGE ( 'NONE', *, *, #3039, .T. ) ;
#6317 = CYLINDRICAL_SURFACE ( 'NONE', #12987, 7.500000000000000888 ) ;
#6318 = AXIS2_PLACEMENT_3D ( 'NONE', #8496, #9598, #10823 ) ;
#6319 = LINE ( 'NONE', #4221, #7354 ) ;
#6320 = FACE_OUTER_BOUND ( 'NONE', #12526, .T. ) ;
#6321 = DIRECTION ( 'NONE',  ( 0.000000000000000000, -0.5000000000000011102, -0.8660254037844379305 ) ) ;
#6322 = CARTESIAN_POINT ( 'NONE',  ( 56.30877334542961421, 51.00051614449765935, 0.02388180880515774693 ) ) ;
#6323 = CARTESIAN_POINT ( 'NONE',  ( 54.13287192849671214, 58.70051614449765509, -5.649768623646139964 ) ) ;
#6324 = CARTESIAN_POINT ( 'NONE',  ( 54.68390685589033495, 47.69948385550240744, -6.485486291978119766 ) ) ;
#6325 = EDGE_CURVE ( 'NONE', #3166, #3701, #2866, .T. ) ;
#6326 = CARTESIAN_POINT ( 'NONE',  ( -4.000000000000000000, -2.472261339043343220, -3.687027428081192326 ) ) ;
#6327 = CARTESIAN_POINT ( 'NONE',  ( 41.58830220609386430, 54.00051614449765935, -0.02388180880514929535 ) ) ;
#6328 = ORIENTED_EDGE ( 'NONE', *, *, #5701, .F. ) ;
#6329 = ORIENTED_EDGE ( 'NONE', *, *, #9559, .F. ) ;
#6330 = ORIENTED_EDGE ( 'NONE', *, *, #8914, .T. ) ;
#6331 = PLANE ( 'NONE',  #2710 ) ;
#6332 = FACE_OUTER_BOUND ( 'NONE', #7796, .T. ) ;
#6333 = DIRECTION ( 'NONE',  ( 0.000000000000000000, 0.000000000000000000, 1.000000000000000000 ) ) ;
#6334 = CARTESIAN_POINT ( 'NONE',  ( -1.575481281892997891E-16, 0.4887495715076908831, -5.000000000000000000 ) ) ;
#6335 = CARTESIAN_POINT ( 'NONE',  ( 46.45491332379572924, 51.29948385550240175, -4.840751629271157874 ) ) ;
#6336 = CARTESIAN_POINT ( 'NONE',  ( -12.17636723815377309, -28.75991329190052070, 0.000000000000000000 ) ) ;
#6337 = CARTESIAN_POINT ( 'NONE',  ( 56.79116909180259398, 49.20051614449766220, 4.963592699178938972 ) ) ;
#6338 = CIRCLE ( 'NONE', #1972, 5.000000000000000888 ) ;
#6339 = CARTESIAN_POINT ( 'NONE',  ( 20.00000000000000000, -20.00000000000000000, -10.79827876554711530 ) ) ;
#6340 = CARTESIAN_POINT ( 'NONE',  ( 1.925929944387235853E-31, 15.00000000000001599, 15.00000000000000000 ) ) ;
#6341 = DIRECTION ( 'NONE',  ( 0.000000000000000000, 0.000000000000000000, -1.000000000000000000 ) ) ;
#6342 = CARTESIAN_POINT ( 'NONE',  ( 44.05948171654945611, 56.20051614449764799, -4.345558710429044069 ) ) ;
#6343 = CARTESIAN_POINT ( 'NONE',  ( 51.92680522751233951, 59.59948385550240602, -6.007379884777223289 ) ) ;
#6344 = DIRECTION ( 'NONE',  ( -1.000000000000000000, 0.000000000000000000, 0.000000000000000000 ) ) ;
#6345 = ORIENTED_EDGE ( 'NONE', *, *, #11577, .T. ) ;
#6346 = CARTESIAN_POINT ( 'NONE',  ( 0.000000000000000000, 0.000000000000000000, 0.000000000000000000 ) ) ;
#6347 = ORIENTED_EDGE ( 'NONE', *, *, #3344, .T. ) ;
#6348 = CARTESIAN_POINT ( 'NONE',  ( 2.449293598294706513E-15, -20.00000000000000000, 9.000000000000000000 ) ) ;
#6349 = EDGE_CURVE ( 'NONE', #11021, #9950, #6278, .T. ) ;
#6350 = PRODUCT_DEFINITION_SHAPE ( 'NONE', 'NONE',  #13673 ) ;
#6351 = CARTESIAN_POINT ( 'NONE',  ( -6.165086708099452473, -33.67449106481171128, 0.000000000000000000 ) ) ;
#6352 = CARTESIAN_POINT ( 'NONE',  ( 6.207541730803228575, -1.039448978216581665, 5.000000000000000888 ) ) ;
#6353 =( GEOMETRIC_REPRESENTATION_CONTEXT ( 3 ) GLOBAL_UNCERTAINTY_ASSIGNED_CONTEXT ( ( #4032 ) ) GLOBAL_UNIT_ASSIGNED_CONTEXT ( ( #7764, #2630, #12177 ) ) REPRESENTATION_CONTEXT ( 'NONE', 'WORKASPACE' ) );
#6354 =( LENGTH_UNIT ( ) NAMED_UNIT ( * ) SI_UNIT ( .MILLI., .METRE. ) );
#6355 = CARTESIAN_POINT ( 'NONE',  ( 50.02271294988512551, 48.49948385550240459, 7.000000000000000888 ) ) ;
#6356 = DIRECTION ( 'NONE',  ( 0.000000000000000000, 0.000000000000000000, 1.000000000000000000 ) ) ;
#6357 = CARTESIAN_POINT ( 'NONE',  ( 48.07319477248762496, 54.40051614449765793, -6.007379884777208190 ) ) ;
#6358 = CARTESIAN_POINT ( 'NONE',  ( 75.00000000000001421, -7.499999999999971578, -20.00000000000000000 ) ) ;
#6359 = CARTESIAN_POINT ( 'NONE',  ( 55.96859303347804371, 64.19948385550239323, 4.306917132069425946 ) ) ;
#6360 = CARTESIAN_POINT ( 'NONE',  ( 45.90387839640214196, 64.69948385550240744, 5.676469297603166098 ) ) ;
#6361 = CARTESIAN_POINT ( 'NONE',  ( 52.29715082351547295, 62.39948385550239607, 6.992620115222774047 ) ) ;
#6362 = ORIENTED_EDGE ( 'NONE', *, *, #12656, .F. ) ;
#6363 = ORIENTED_EDGE ( 'NONE', *, *, #5252, .F. ) ;
#6364 = DIRECTION ( 'NONE',  ( 0.000000000000000000, 0.000000000000000000, -1.000000000000000000 ) ) ;
#6365 = CARTESIAN_POINT ( 'NONE',  ( 0.3106000600989247684, -3.122278952918441597, 4.592054218142290978 ) ) ;
#6366 = DIRECTION ( 'NONE',  ( -1.000000000000000000, 0.000000000000000000, -0.000000000000000000 ) ) ;
#6367 = PLANE ( 'NONE',  #4972 ) ;
#6368 = CARTESIAN_POINT ( 'NONE',  ( 47.70284917648453415, 47.39948385550239607, -6.992620115222774047 ) ) ;
#6369 = CARTESIAN_POINT ( 'NONE',  ( 44.05948171654945611, 48.20051614449764799, -4.345558710429044069 ) ) ;
#6370 = FACE_OUTER_BOUND ( 'NONE', #10300, .T. ) ;
#6371 = ADVANCED_FACE ( 'NONE', ( #10330 ), #8448, .F. ) ;
#6372 = CARTESIAN_POINT ( 'NONE',  ( 56.65037692655918988, 45.89948385550240317, -2.184720259617163762 ) ) ;
#6373 = CARTESIAN_POINT ( 'NONE',  ( 4.078421086530217288, -3.990950201428958621, -1.000000000000000000 ) ) ;
#6374 = CARTESIAN_POINT ( 'NONE',  ( 52.62207051974839089, 58.39948385550241028, 7.992620115222770494 ) ) ;
#6375 = EDGE_LOOP ( 'NONE', ( #633, #3436, #199, #6314 ) ) ;
#6376 = ORIENTED_EDGE ( 'NONE', *, *, #12335, .F. ) ;
#6377 = CARTESIAN_POINT ( 'NONE',  ( 62.50000000000000000, 20.00000000000001421, 9.999999999999998224 ) ) ;
#6378 = EDGE_CURVE ( 'NONE', #9857, #11796, #5233, .T. ) ;
#6379 = EDGE_CURVE ( 'NONE', #11927, #2163, #1133, .T. ) ;
#6380 = VECTOR ( 'NONE', #2419, 999.9999999999998863 ) ;
#6381 = CARTESIAN_POINT ( 'NONE',  ( 9.999999999999994671, 20.00000000000001421, 9.999999999999998224 ) ) ;
#6382 = CARTESIAN_POINT ( 'NONE',  ( 2.449293598294706513E-15, -20.00000000000000000, 9.000000000000000000 ) ) ;
#6383 = CARTESIAN_POINT ( 'NONE',  ( -74.99999999999998579, 7.499999999999975131, 10.00000000000000000 ) ) ;
#6384 = CARTESIAN_POINT ( 'NONE',  ( 55.08986747509849380, 45.20051614449766220, 3.727524721679155384 ) ) ;
#6385 = CARTESIAN_POINT ( 'NONE',  ( 45.90387839640208512, 60.30051614449766362, -5.676469297603124353 ) ) ;
#6386 = CARTESIAN_POINT ( 'NONE',  ( 43.18075615816994173, 63.80051614449766362, 4.924951120819380357 ) ) ;
#6387 = CARTESIAN_POINT ( 'NONE',  ( 4.170895651974851681, -4.109780709045220526, -1.251026243406537913E-13 ) ) ;
#6388 = CARTESIAN_POINT ( 'NONE',  ( 52.57664461997821093, 57.40051614449767214, 8.007379884777206414 ) ) ;
#6389 = APPLICATION_CONTEXT ( 'automotive_design' ) ;
#6390 = ORIENTED_EDGE ( 'NONE', *, *, #8708, .T. ) ;
#6391 = CIRCLE ( 'NONE', #1281, 4.000000000000000000 ) ;
#6392 = VERTEX_POINT ( 'NONE', #5297 ) ;
#6393 = ORIENTED_EDGE ( 'NONE', *, *, #10737, .F. ) ;
#6394 = DIRECTION ( 'NONE',  ( -0.000000000000000000, -0.000000000000000000, -1.000000000000000000 ) ) ;
#6395 = EDGE_CURVE ( 'NONE', #2677, #13245, #1357, .T. ) ;
#6396 = CARTESIAN_POINT ( 'NONE',  ( 6.385552186430389021, 2.886751345948122438, -5.000000000000001776 ) ) ;
#6397 = DIRECTION ( 'NONE',  ( -1.000000000000000000, 0.000000000000000000, 0.000000000000000000 ) ) ;
#6398 = DIRECTION ( 'NONE',  ( -0.000000000000000000, -0.000000000000000000, -1.000000000000000000 ) ) ;
#6399 = DIRECTION ( 'NONE',  ( 0.000000000000000000, 0.000000000000000000, -1.000000000000000000 ) ) ;
#6400 = CARTESIAN_POINT ( 'NONE',  ( 55.08986747509847248, 47.79948385550240886, -3.727524721679197572 ) ) ;
#6401 = VECTOR ( 'NONE', #11590, 1000.000000000000000 ) ;
#6402 = CARTESIAN_POINT ( 'NONE',  ( -2.100000000000000089, 2.571758278209441957E-16, -5.000000000000000000 ) ) ;
#6403 = CARTESIAN_POINT ( 'NONE',  ( 52.57664461997821093, 47.40051614449765793, 8.007379884777206414 ) ) ;
#6404 = AXIS2_PLACEMENT_3D ( 'NONE', #627, #3764, #4881 ) ;
#6405 = DIRECTION ( 'NONE',  ( 0.000000000000000000, 0.5000000000000011102, 0.8660254037844379305 ) ) ;
#6406 = DIRECTION ( 'NONE',  ( 0.000000000000000000, -0.8660254037844391517, -0.4999999999999991673 ) ) ;
#6407 = EDGE_CURVE ( 'NONE', #5893, #2278, #4044, .T. ) ;
#6408 = CARTESIAN_POINT ( 'NONE',  ( 52.25172492374527877, 59.40051614449765083, 7.007379884777203749 ) ) ;
#6409 = CARTESIAN_POINT ( 'NONE',  ( 55.69932041026404335, 59.89948385550240317, -1.875703265242203432 ) ) ;
#6410 = CARTESIAN_POINT ( 'NONE',  ( 12.99038105676665289, -27.49999999999988276, -9.000000000000000000 ) ) ;
#6411 = ORIENTED_EDGE ( 'NONE', *, *, #13008, .T. ) ;
#6412 = DIRECTION ( 'NONE',  ( 0.000000000000000000, 0.000000000000000000, -1.000000000000000000 ) ) ;
#6413 = EDGE_LOOP ( 'NONE', ( #5720, #12993, #3349, #8543, #6074 ) ) ;
#6414 = CARTESIAN_POINT ( 'NONE',  ( -19.99999999999999289, -14.99999999999998579, -23.00000000000000000 ) ) ;
#6415 = DIRECTION ( 'NONE',  ( 0.000000000000000000, -0.000000000000000000, 1.000000000000000000 ) ) ;
#6416 = CARTESIAN_POINT ( 'NONE',  ( 4.082498951862918446, 2.020725942163685396, -3.500000000000001332 ) ) ;
#6417 = CARTESIAN_POINT ( 'NONE',  ( 56.66441430157296821, 54.09948385550240602, 2.141517661632100111 ) ) ;
#6418 = CARTESIAN_POINT ( 'NONE',  ( 43.20883090819745576, 58.79948385550240175, 4.963592699179006473 ) ) ;
#6419 = AXIS2_PLACEMENT_3D ( 'NONE', #3356, #2310, #12813 ) ;
#6420 = B_SPLINE_CURVE_WITH_KNOTS ( 'NONE', 3,
 ( #9510, #7572, #9441, #10612, #10477, #4257, #5241, #11713, #5373, #3350, #8413, #235, #9577, #12551, #4190, #4451 ),
 .UNSPECIFIED., .F., .F.,
 ( 4, 3, 3, 3, 3, 4 ),
 ( 0.000000000000000000, 5.303647860849292387E-05, 0.0001057093501027219331, 0.0001642058037231606204, 0.0002210073443958821807, 0.0002236769549542877021 ),
 .UNSPECIFIED. ) ;
#6421 = CARTESIAN_POINT ( 'NONE',  ( 4.071447262713888016, -2.020725942163694722, -3.499999999999999556 ) ) ;
#6422 = CARTESIAN_POINT ( 'NONE',  ( 44.88205777487401349, 51.80051614449766362, 3.688883143319584779 ) ) ;
#6423 = CARTESIAN_POINT ( 'NONE',  ( 0.000000000000000000, 0.000000000000000000, -3.499999999999999556 ) ) ;
#6424 = CARTESIAN_POINT ( 'NONE',  ( 54.13287192849676188, 64.29948385550241596, 5.649768623646098220 ) ) ;
#6425 = CARTESIAN_POINT ( 'NONE',  ( 6.533910050139697390, -5.901028503456124064, 1.992084869049455159E-14 ) ) ;
#6426 = CARTESIAN_POINT ( 'NONE',  ( 43.34962307344081012, 60.89948385550241028, 2.184720259617164650 ) ) ;
#6427 = VERTEX_POINT ( 'NONE', #13570 ) ;
#6428 = ORIENTED_EDGE ( 'NONE', *, *, #7806, .T. ) ;
#6429 = CARTESIAN_POINT ( 'NONE',  ( -2.836893136758495970, -3.208949435745868328, -3.505054077164885484 ) ) ;
#6430 = AXIS2_PLACEMENT_3D ( 'NONE', #12879, #8549, #12744 ) ;
#6431 = CARTESIAN_POINT ( 'NONE',  ( -6.259644161404860030E-16, -4.618802153517027165, -5.000000000000000000 ) ) ;
#6432 = CARTESIAN_POINT ( 'NONE',  ( 3.974175853610083742, -3.450041667725777472, 1.156004144284040303 ) ) ;
#6433 = DIRECTION ( 'NONE',  ( -1.000000000000000000, -0.000000000000000000, -0.000000000000000000 ) ) ;
#6434 = CARTESIAN_POINT ( 'NONE',  ( 47.74827507625477807, 50.59948385550239891, 7.007379884777229506 ) ) ;
#6435 = CARTESIAN_POINT ( 'NONE',  ( 47.70284917648459100, 45.60051614449765367, 6.992620115222796251 ) ) ;
#6436 = DIRECTION ( 'NONE',  ( -0.000000000000000000, 0.000000000000000000, 1.000000000000000000 ) ) ;
#6437 = CARTESIAN_POINT ( 'NONE',  ( 54.68390685589033495, 63.69948385550240033, -6.485486291978119766 ) ) ;
#6438 = AXIS2_PLACEMENT_3D ( 'NONE', #3047, #8513, #12649 ) ;
#6439 = CARTESIAN_POINT ( 'NONE',  ( 42.39856655714566358, 54.89948385550240317, 2.493737253992119207 ) ) ;
#6440 = EDGE_CURVE ( 'NONE', #11340, #486, #1572, .T. ) ;
#6441 = ORIENTED_EDGE ( 'NONE', *, *, #6132, .T. ) ;
#6442 = ORIENTED_EDGE ( 'NONE', *, *, #8224, .T. ) ;
#6443 = DIRECTION ( 'NONE',  ( 0.000000000000000000, 1.000000000000000000, 0.000000000000000000 ) ) ;
#6444 = VECTOR ( 'NONE', #7174, 1000.000000000000000 ) ;
#6445 = CARTESIAN_POINT ( 'NONE',  ( 6.541334219041335274, -2.934241909852036478, 5.143243597038029691 ) ) ;
#6446 = DIRECTION ( 'NONE',  ( -0.000000000000000000, -0.000000000000000000, 1.000000000000000000 ) ) ;
#6447 = CARTESIAN_POINT ( 'NONE',  ( 44.88205777487401349, 45.80051614449766362, 3.688883143319584779 ) ) ;
#6448 = CARTESIAN_POINT ( 'NONE',  ( 52.29715082351539479, 60.60051614449764656, -6.992620115222796251 ) ) ;
#6449 = EDGE_CURVE ( 'NONE', #6051, #6095, #981, .T. ) ;
#6450 = CARTESIAN_POINT ( 'NONE',  ( 49.97728705011486738, 45.49948385550240459, -8.000000000000001776 ) ) ;
#6451 = EDGE_CURVE ( 'NONE', #9726, #9705, #2637, .T. ) ;
#6452 = CARTESIAN_POINT ( 'NONE',  ( 0.000000000000000000, 0.8865213383406715941, 1.535499999999999199 ) ) ;
#6453 = EDGE_CURVE ( 'NONE', #9858, #5442, #7234, .T. ) ;
#6454 = CARTESIAN_POINT ( 'NONE',  ( 42.38452918213190657, 53.90051614449765793, 2.450534656007115508 ) ) ;
#6455 = AXIS2_PLACEMENT_3D ( 'NONE', #6661, #10991, #1513 ) ;
#6456 = ADVANCED_FACE ( 'NONE', ( #9370 ), #2271, .F. ) ;
#6457 = VECTOR ( 'NONE', #12933, 1000.000000000000114 ) ;
#6458 = ORIENTED_EDGE ( 'NONE', *, *, #5956, .T. ) ;
#6459 = EDGE_LOOP ( 'NONE', ( #10228, #8013, #1861, #3056 ) ) ;
#6460 = EDGE_LOOP ( 'NONE', ( #10337, #4069, #2697, #10247 ) ) ;
#6461 = DIRECTION ( 'NONE',  ( 9.858538378746663627E-23, -5.031452844637890958E-23, 1.000000000000000000 ) ) ;
#6462 = LINE ( 'NONE', #11766, #6938 ) ;
#6463 = CARTESIAN_POINT ( 'NONE',  ( -4.024497503033519941, -2.323544716729390558, -3.572167766733381544 ) ) ;
#6464 = VECTOR ( 'NONE', #3740, 1000.000000000000000 ) ;
#6465 = CARTESIAN_POINT ( 'NONE',  ( 48.02776887271745210, 51.39948385550241028, -5.992620115222778487 ) ) ;
#6466 = CONICAL_SURFACE ( 'NONE', #6899, 1.999999999999998224, 1.029744259999999745 ) ;
#6467 = CARTESIAN_POINT ( 'NONE',  ( 49.97728705011488159, 65.49948385550240459, -7.000000000000000888 ) ) ;
#6468 = CARTESIAN_POINT ( 'NONE',  ( 47.74827507625469281, 64.40051614449765793, -7.007379884777203749 ) ) ;
#6469 = DIRECTION ( 'NONE',  ( -0.000000000000000000, -0.000000000000000000, -1.000000000000000000 ) ) ;
#6470 = DIRECTION ( 'NONE',  ( 0.000000000000000000, 0.000000000000000000, -1.000000000000000000 ) ) ;
#6471 = CARTESIAN_POINT ( 'NONE',  ( 55.94051828345053679, 55.20051614449766930, 4.345558710429044069 ) ) ;
#6472 = CARTESIAN_POINT ( 'NONE',  ( 44.91013252490152752, 60.79948385550241596, 3.727524721679198461 ) ) ;
#6473 = CARTESIAN_POINT ( 'NONE',  ( -62.49999999999997158, 45.00000000000001421, 15.00000000000000000 ) ) ;
#6474 = EDGE_CURVE ( 'NONE', #9060, #4066, #13055, .T. ) ;
#6475 = ORIENTED_EDGE ( 'NONE', *, *, #4899, .T. ) ;
#6476 = VECTOR ( 'NONE', #12144, 1000.000000000000000 ) ;
#6477 = CARTESIAN_POINT ( 'NONE',  ( 2.290893957444128645E-15, 4.647089433458768681, -3.572167766733382877 ) ) ;
#6478 = VERTEX_POINT ( 'NONE', #4996 ) ;
#6479 = DIRECTION ( 'NONE',  ( 1.000000000000000000, 0.000000000000000000, 0.000000000000000000 ) ) ;
#6480 = AXIS2_PLACEMENT_3D ( 'NONE', #5903, #7969, #11140 ) ;
#6481 = DIRECTION ( 'NONE',  ( -0.000000000000000000, 0.000000000000000000, -1.000000000000000000 ) ) ;
#6482 = DIRECTION ( 'NONE',  ( -1.000000000000000000, 1.734723475976807094E-16, 0.000000000000000000 ) ) ;
#6483 = DIRECTION ( 'NONE',  ( 1.000000000000000000, 0.000000000000000000, 0.000000000000000000 ) ) ;
#6484 = CARTESIAN_POINT ( 'NONE',  ( 44.05948171654949874, 52.79948385550240175, 4.345558710429105354 ) ) ;
#6485 = FACE_OUTER_BOUND ( 'NONE', #11128, .T. ) ;
#6486 = CARTESIAN_POINT ( 'NONE',  ( 55.08986747509849380, 49.20051614449766220, 3.727524721679155384 ) ) ;
#6487 = DIRECTION ( 'NONE',  ( -0.000000000000000000, -0.000000000000000000, -1.000000000000000000 ) ) ;
#6488 = CARTESIAN_POINT ( 'NONE',  ( 4.000000000000000000, -1.942223658245635809, -0.3516579909967643691 ) ) ;
#6489 = EDGE_CURVE ( 'NONE', #9824, #1019, #1794, .T. ) ;
#6490 = DIRECTION ( 'NONE',  ( 1.000000000000000000, 0.000000000000000000, 0.000000000000000000 ) ) ;
#6491 = CARTESIAN_POINT ( 'NONE',  ( 45.90387839640214196, 58.69948385550240033, 5.676469297603166098 ) ) ;
#6492 = CIRCLE ( 'NONE', #12428, 5.000000000000000888 ) ;
#6493 = CARTESIAN_POINT ( 'NONE',  ( 0.05140428708382910328, -4.819072548984009607, -1.653121499799246719 ) ) ;
#6494 = VERTEX_POINT ( 'NONE', #812 ) ;
#6495 = UNCERTAINTY_MEASURE_WITH_UNIT (LENGTH_MEASURE( 1.000000000000000082E-05 ), #3267, 'distance_accuracy_value', 'NONE');
#6496 = ORIENTED_EDGE ( 'NONE', *, *, #4413, .F. ) ;
#6497 = EDGE_LOOP ( 'NONE', ( #7756, #5483, #6623, #8978, #13377, #12821, #2731, #13203, #6583, #12753, #1471, #11164 ) ) ;
#6498 = CARTESIAN_POINT ( 'NONE',  ( 4.124214193018070240, 4.056676826581888662, 1.068854115921270076E-15 ) ) ;
#6499 = CONICAL_SURFACE ( 'NONE', #4716, 3.309499999999999886, 0.7853981633974407295 ) ;
#6500 = CARTESIAN_POINT ( 'NONE',  ( 1.171083334267915221, -24.65495046420793201, 9.999999999999998224 ) ) ;
#6501 = CARTESIAN_POINT ( 'NONE',  ( 3.972066048304701891, -2.740530939476090388, 2.384802634787825504 ) ) ;
#6502 = LINE ( 'NONE', #7528, #8056 ) ;
#6503 = CARTESIAN_POINT ( 'NONE',  ( 44.03140696652193498, 55.19948385550240744, -4.306917132069424170 ) ) ;
#6504 = CARTESIAN_POINT ( 'NONE',  ( 55.94051828345053679, 55.20051614449766930, 4.345558710429044069 ) ) ;
#6505 = CARTESIAN_POINT ( 'NONE',  ( -0.9999999999999976685, -20.00000000000000000, -9.000000000000001776 ) ) ;
#6506 = CARTESIAN_POINT ( 'NONE',  ( 45.90387839640214196, 48.69948385550240744, 5.676469297603166098 ) ) ;
#6507 = FILL_AREA_STYLE_COLOUR ( '', #13644 ) ;
#6508 = CARTESIAN_POINT ( 'NONE',  ( 57.60143344285433642, 55.89948385550241028, -2.493737253992118319 ) ) ;
#6509 = CIRCLE ( 'NONE', #513, 0.7500000000000000000 ) ;
#6510 = ORIENTED_EDGE ( 'NONE', *, *, #2738, .F. ) ;
#6511 = ORIENTED_EDGE ( 'NONE', *, *, #4819, .F. ) ;
#6512 = CYLINDRICAL_SURFACE ( 'NONE', #3199, 7.500000000000000888 ) ;
#6513 = AXIS2_PLACEMENT_3D ( 'NONE', #6954, #5995, #9094 ) ;
#6514 = CARTESIAN_POINT ( 'NONE',  ( -4.078421086530219064, -3.990950201428956845, 0.000000000000000000 ) ) ;
#6515 = CARTESIAN_POINT ( 'NONE',  ( 48.02776887271750184, 47.60051614449766078, 5.992620115222795363 ) ) ;
#6516 = CARTESIAN_POINT ( 'NONE',  ( -0.9999999999999995559, -15.10102051443364246, 9.000000000000000000 ) ) ;
#6517 = CIRCLE ( 'NONE', #8283, 1.499999999999999334 ) ;
#6518 = CARTESIAN_POINT ( 'NONE',  ( 47.42335538002188144, 48.59948385550239891, 8.007379884777233059 ) ) ;
#6519 = CARTESIAN_POINT ( 'NONE',  ( 3.950241966888466738, 2.668221755853590782, 2.378504353001025695 ) ) ;
#6520 = VECTOR ( 'NONE', #13221, 1000.000000000000000 ) ;
#6521 = CARTESIAN_POINT ( 'NONE',  ( 42.38452918213190657, 55.90051614449766504, 2.450534656007115508 ) ) ;
#6522 = ORIENTED_EDGE ( 'NONE', *, *, #2576, .F. ) ;
#6523 = ORIENTED_EDGE ( 'NONE', *, *, #3908, .F. ) ;
#6524 = ORIENTED_EDGE ( 'NONE', *, *, #9063, .T. ) ;
#6525 = ORIENTED_EDGE ( 'NONE', *, *, #10359, .T. ) ;
#6526 = VECTOR ( 'NONE', #12710, 1000.000000000000000 ) ;
#6527 = DIRECTION ( 'NONE',  ( 1.049727191973306010E-16, 0.5150380737757248584, -0.8571673013836862420 ) ) ;
#6528 = DIRECTION ( 'NONE',  ( 0.000000000000000000, 0.000000000000000000, -1.000000000000000000 ) ) ;
#6529 = DIRECTION ( 'NONE',  ( -0.000000000000000000, -0.000000000000000000, 1.000000000000000000 ) ) ;
#6530 = DIRECTION ( 'NONE',  ( 0.000000000000000000, 1.776356839400250465E-15, -1.000000000000000000 ) ) ;
#6531 = CARTESIAN_POINT ( 'NONE',  ( 55.69932041026404335, 49.89948385550241028, -1.875703265242203432 ) ) ;
#6532 = DIRECTION ( 'NONE',  ( -0.000000000000000000, 1.000000000000000000, -0.000000000000000000 ) ) ;
#6533 = CARTESIAN_POINT ( 'NONE',  ( 47.37792948025170858, 45.60051614449765367, 7.992620115222797139 ) ) ;
#6534 = DIRECTION ( 'NONE',  ( 0.000000000000000000, 0.5000000000000018874, 0.8660254037844375974 ) ) ;
#6535 = CARTESIAN_POINT ( 'NONE',  ( -3.114822491369819039E-15, 4.452621892014636096, 2.287832656137190668 ) ) ;
#6536 = CARTESIAN_POINT ( 'NONE',  ( 55.96859303347802239, 56.80051614449764230, -4.306917132069484566 ) ) ;
#6537 = CARTESIAN_POINT ( 'NONE',  ( 44.30067958973596376, 58.89948385550241028, 1.875703265242204099 ) ) ;
#6538 = ORIENTED_EDGE ( 'NONE', *, *, #1272, .F. ) ;
#6539 = DIRECTION ( 'NONE',  ( -1.000000000000000000, 0.000000000000000000, 0.000000000000000000 ) ) ;
#6540 = ORIENTED_EDGE ( 'NONE', *, *, #6620, .T. ) ;
#6541 = DIRECTION ( 'NONE',  ( 3.469446951953615175E-16, -1.000000000000000000, 0.000000000000000000 ) ) ;
#6542 = DIRECTION ( 'NONE',  ( -1.000000000000000000, -0.000000000000000000, -0.000000000000000000 ) ) ;
#6543 = DIRECTION ( 'NONE',  ( -0.000000000000000000, -0.000000000000000000, 1.000000000000000000 ) ) ;
#6544 = EDGE_CURVE ( 'NONE', #2116, #13409, #6925, .T. ) ;
#6545 = EDGE_CURVE ( 'NONE', #13432, #5283, #10234, .T. ) ;
#6546 =( NAMED_UNIT ( * ) PLANE_ANGLE_UNIT ( ) SI_UNIT ( $, .RADIAN. ) );
#6547 = CARTESIAN_POINT ( 'NONE',  ( 47.74827507625478518, 48.59948385550239180, 7.007379884777227730 ) ) ;
#6548 = ADVANCED_FACE ( 'NONE', ( #7963 ), #4926, .F. ) ;
#6549 = CYLINDRICAL_SURFACE ( 'NONE', #10607, 15.00000000000000000 ) ;
#6550 = CARTESIAN_POINT ( 'NONE',  ( 44.91013252490150620, 50.20051614449766220, -3.727524721679154940 ) ) ;
#6551 = CARTESIAN_POINT ( 'NONE',  ( -6.000000000000012434, -7.009618943233427935, 9.000000000000000000 ) ) ;
#6552 = CARTESIAN_POINT ( 'NONE',  ( 6.355827204229362870, 3.436818823786758070, 4.264647808192652434 ) ) ;
#6553 = CARTESIAN_POINT ( 'NONE',  ( 57.36023556966787851, 61.99948385550241170, -0.02388180880522424582 ) ) ;
#6554 = CARTESIAN_POINT ( 'NONE',  ( 0.000000000000000000, 0.000000000000000000, 0.000000000000000000 ) ) ;
#6555 = ORIENTED_EDGE ( 'NONE', *, *, #9443, .F. ) ;
#6556 = AXIS2_PLACEMENT_3D ( 'NONE', #4805, #8125, #1466 ) ;
#6557 = VERTEX_POINT ( 'NONE', #12243 ) ;
#6558 = CARTESIAN_POINT ( 'NONE',  ( 4.170895651974850793, 4.109780709045216085, 3.964526709274768569E-16 ) ) ;
#6559 = AXIS2_PLACEMENT_3D ( 'NONE', #3613, #3473, #11831 ) ;
#6560 = CARTESIAN_POINT ( 'NONE',  ( 0.05140428708382505096, -3.841181488860373250, 3.346878500200758833 ) ) ;
#6561 = CARTESIAN_POINT ( 'NONE',  ( 3.973110223767137850, -2.261493176400255405E-11, -3.565797985667433334 ) ) ;
#6562 = FACE_BOUND ( 'NONE', #6071, .T. ) ;
#6563 = CARTESIAN_POINT ( 'NONE',  ( 54.09612160359786515, 49.69948385550240744, -5.676469297603166098 ) ) ;
#6564 = CARTESIAN_POINT ( 'NONE',  ( 52.29715082351538769, 56.60051614449766788, -6.992620115222796251 ) ) ;
#6565 = PRODUCT_DEFINITION_SHAPE ( 'NONE', 'NONE',  #12073 ) ;
#6566 = CARTESIAN_POINT ( 'NONE',  ( -14.99999999999999645, -20.00000000000005329, 9.000000000000000000 ) ) ;
#6567 = CARTESIAN_POINT ( 'NONE',  ( 47.70284917648453415, 53.39948385550238186, -6.992620115222774047 ) ) ;
#6568 = CARTESIAN_POINT ( 'NONE',  ( 30.00000000000000355, 40.00000000000000000, -9.999999999999998224 ) ) ;
#6569 = ADVANCED_FACE ( 'NONE', ( #12378 ), #9138, .T. ) ;
#6570 = CARTESIAN_POINT ( 'NONE',  ( 58.41169779390614281, 63.99948385550241170, -0.02388180880523160798 ) ) ;
#6571 = VERTEX_POINT ( 'NONE', #1867 ) ;
#6572 = ORIENTED_EDGE ( 'NONE', *, *, #12713, .F. ) ;
#6573 = LINE ( 'NONE', #5407, #9607 ) ;
#6574 = EDGE_CURVE ( 'NONE', #919, #11844, #5967, .T. ) ;
#6575 = DIRECTION ( 'NONE',  ( 0.000000000000000000, 0.000000000000000000, -1.000000000000000000 ) ) ;
#6576 = CARTESIAN_POINT ( 'NONE',  ( 48.02776887271750184, 51.60051614449766788, 5.992620115222795363 ) ) ;
#6577 = CARTESIAN_POINT ( 'NONE',  ( 56.65037692655921120, 63.10051614449766078, 2.184720259617097593 ) ) ;
#6578 = CARTESIAN_POINT ( 'NONE',  ( 42.39856655714566358, 54.89948385550240317, 2.493737253992119207 ) ) ;
#6579 = CARTESIAN_POINT ( 'NONE',  ( 44.03140696652192787, 55.19948385550238612, -4.306917132069425058 ) ) ;
#6580 = DIRECTION ( 'NONE',  ( 0.000000000000000000, 0.000000000000000000, 1.000000000000000000 ) ) ;
#6581 = CARTESIAN_POINT ( 'NONE',  ( 47.37792948025170858, 57.60051614449765367, 7.992620115222797139 ) ) ;
#6582 = ORIENTED_EDGE ( 'NONE', *, *, #2536, .F. ) ;
#6583 = ORIENTED_EDGE ( 'NONE', *, *, #4202, .F. ) ;
#6584 = VERTEX_POINT ( 'NONE', #6996 ) ;
#6585 = VECTOR ( 'NONE', #3100, 1000.000000000000000 ) ;
#6586 = VERTEX_POINT ( 'NONE', #7137 ) ;
#6587 = PRODUCT_DEFINITION ( 'UNKNOWN', '', #3526, #12137 ) ;
#6588 = DIRECTION ( 'NONE',  ( 0.000000000000000000, 0.000000000000000000, -1.000000000000000000 ) ) ;
#6589 = PRESENTATION_STYLE_ASSIGNMENT (( #1374 ) ) ;
#6590 =( LENGTH_UNIT ( ) NAMED_UNIT ( * ) SI_UNIT ( .MILLI., .METRE. ) );
#6591 = CARTESIAN_POINT ( 'NONE',  ( 14.92500000000001492, -21.49812382665770727, 0.000000000000000000 ) ) ;
#6592 = CARTESIAN_POINT ( 'NONE',  ( 55.08986747509847248, 53.79948385550241596, -3.727524721679197572 ) ) ;
#6593 = CARTESIAN_POINT ( 'NONE',  ( 49.97728705011495265, 49.50051614449765935, 7.000000000000000888 ) ) ;
#6594 = CARTESIAN_POINT ( 'NONE',  ( 52.57664461997821093, 49.40051614449766504, 8.007379884777206414 ) ) ;
#6595 = CARTESIAN_POINT ( 'NONE',  ( 0.3126073911696408136, 2.020725942163688060, 3.500000000000000000 ) ) ;
#6596 = LINE ( 'NONE', #8599, #7366 ) ;
#6597 = CARTESIAN_POINT ( 'NONE',  ( 47.74827507625469281, 56.40051614449766504, -7.007379884777203749 ) ) ;
#6598 = CARTESIAN_POINT ( 'NONE',  ( 51.97223112728254790, 62.39948385550240317, 5.992620115222778487 ) ) ;
#6599 = VERTEX_POINT ( 'NONE', #4853 ) ;
#6600 = CARTESIAN_POINT ( 'NONE',  ( 5.599999999999999645, -2.020725942163694722, -3.499999999999999556 ) ) ;
#6601 = EDGE_CURVE ( 'NONE', #10387, #1211, #11345, .T. ) ;
#6602 = ORIENTED_EDGE ( 'NONE', *, *, #9608, .F. ) ;
#6603 = CARTESIAN_POINT ( 'NONE',  ( 0.000000000000000000, 0.000000000000000000, 0.000000000000000000 ) ) ;
#6604 = CIRCLE ( 'NONE', #7272, 0.7500000000000000000 ) ;
#6605 = DIRECTION ( 'NONE',  ( -1.000000000000000000, -0.000000000000000000, -0.000000000000000000 ) ) ;
#6606 = CARTESIAN_POINT ( 'NONE',  ( 3.973514160553461849, 2.741076955031360285, 2.383932505289871884 ) ) ;
#6607 = CARTESIAN_POINT ( 'NONE',  ( 56.66441430157296821, 50.09948385550240602, 2.141517661632100111 ) ) ;
#6608 = CARTESIAN_POINT ( 'NONE',  ( 1.393927851585479161, -4.043713361053543842, -3.526374918436840922 ) ) ;
#6609 = CARTESIAN_POINT ( 'NONE',  ( 55.11794222512599362, 58.80051614449766362, -3.688883143319583446 ) ) ;
#6610 = EDGE_CURVE ( 'NONE', #245, #13024, #4785, .T. ) ;
#6611 = LINE ( 'NONE', #304, #11537 ) ;
#6612 = COLOUR_RGB ( '',0.8941176470588234615, 0.8941176470588234615, 0.8941176470588234615 ) ;
#6613 = CARTESIAN_POINT ( 'NONE',  ( 6.371506350351446635, 5.409331239960136983, 0.8483282427581467777 ) ) ;
#6614 = CARTESIAN_POINT ( 'NONE',  ( 6.506987859255521478, -5.850751062354593302, 2.176274696337492837E-17 ) ) ;
#6615 = CARTESIAN_POINT ( 'NONE',  ( 48.07319477248768180, 46.59948385550239891, 6.007379884777225953 ) ) ;
#6616 = DIRECTION ( 'NONE',  ( 0.000000000000000000, 0.000000000000000000, 1.000000000000000000 ) ) ;
#6617 = AXIS2_PLACEMENT_3D ( 'NONE', #9274, #11410, #1929 ) ;
#6618 = EDGE_CURVE ( 'NONE', #9204, #11968, #11302, .T. ) ;
#6619 = VERTEX_POINT ( 'NONE', #8104 ) ;
#6620 = EDGE_CURVE ( 'NONE', #10838, #11193, #673, .T. ) ;
#6621 = EDGE_CURVE ( 'NONE', #6230, #13042, #5896, .T. ) ;
#6622 = UNCERTAINTY_MEASURE_WITH_UNIT (LENGTH_MEASURE( 1.000000000000000082E-05 ), #2494, 'distance_accuracy_value', 'NONE');
#6623 = ORIENTED_EDGE ( 'NONE', *, *, #4706, .F. ) ;
#6624 = FACE_OUTER_BOUND ( 'NONE', #5982, .T. ) ;
#6625 = DIRECTION ( 'NONE',  ( -1.000000000000000000, 0.000000000000000000, -0.000000000000000000 ) ) ;
#6626 =( GEOMETRIC_REPRESENTATION_CONTEXT ( 3 ) GLOBAL_UNCERTAINTY_ASSIGNED_CONTEXT ( ( #12823 ) ) GLOBAL_UNIT_ASSIGNED_CONTEXT ( ( #7576, #6546, #4527 ) ) REPRESENTATION_CONTEXT ( 'NONE', 'WORKASPACE' ) );
#6627 = CARTESIAN_POINT ( 'NONE',  ( 0.000000000000000000, 0.000000000000000000, 4.000000000000000000 ) ) ;
#6628 = EDGE_CURVE ( 'NONE', #3926, #1542, #8172, .T. ) ;
#6629 = CARTESIAN_POINT ( 'NONE',  ( 4.175813232069146785, 2.061359961916365613, -3.570380186727397653 ) ) ;
#6630 = CARTESIAN_POINT ( 'NONE',  ( 0.000000000000000000, 0.000000000000000000, -1.000000000000000000 ) ) ;
#6631 = CARTESIAN_POINT ( 'NONE',  ( 54.09612160359786515, 51.69948385550240744, -5.676469297603166098 ) ) ;
#6632 = CARTESIAN_POINT ( 'NONE',  ( 45.86712807150329496, 53.70051614449766220, 5.649768623646139964 ) ) ;
#6633 = VECTOR ( 'NONE', #7908, 1000.000000000000000 ) ;
#6634 = DIRECTION ( 'NONE',  ( -1.000000000000000000, 0.000000000000000000, 0.000000000000000000 ) ) ;
#6635 = CARTESIAN_POINT ( 'NONE',  ( 55.96859303347804371, 50.19948385550240744, 4.306917132069425946 ) ) ;
#6636 = FILL_AREA_STYLE ('',( #2330 ) ) ;
#6637 = EDGE_CURVE ( 'NONE', #5736, #4363, #9331, .T. ) ;
#6638 = CARTESIAN_POINT ( 'NONE',  ( 54.72065718078924590, 62.29948385550241596, 6.458785618021043895 ) ) ;
#6639 = AXIS2_PLACEMENT_3D ( 'NONE', #255, #1218, #4480 ) ;
#6640 = ADVANCED_FACE ( 'NONE', ( #2775 ), #13467, .F. ) ;
#6641 = VERTEX_POINT ( 'NONE', #10509 ) ;
#6642 = ORIENTED_EDGE ( 'NONE', *, *, #769, .F. ) ;
#6643 = ORIENTED_EDGE ( 'NONE', *, *, #7030, .F. ) ;
#6644 = CARTESIAN_POINT ( 'NONE',  ( 2.000000000000000000, -0.8865213383406694847, 1.535500000000001419 ) ) ;
#6645 =( REPRESENTATION_RELATIONSHIP ('NONE','NONE', #5328, #8584 ) REPRESENTATION_RELATIONSHIP_WITH_TRANSFORMATION ( #8025 )SHAPE_REPRESENTATION_RELATIONSHIP( ) );
#6646 = LINE ( 'NONE', #3593, #1998 ) ;
#6647 = CARTESIAN_POINT ( 'NONE',  ( 44.30067958973594955, 56.10051614449766078, -1.875703265242155693 ) ) ;
#6648 = CIRCLE ( 'NONE', #6438, 2.649999999999985700 ) ;
#6649 = CARTESIAN_POINT ( 'NONE',  ( -62.49999999999997158, 20.00000000000001421, 15.00000000000000000 ) ) ;
#6650 = CARTESIAN_POINT ( 'NONE',  ( 58.41169779390614281, 51.99948385550239749, -0.02388180880523160798 ) ) ;
#6651 = CARTESIAN_POINT ( 'NONE',  ( 57.36023556966787851, 59.99948385550240459, -0.02388180880522424582 ) ) ;
#6652 = CARTESIAN_POINT ( 'NONE',  ( 4.086376042167606748, 4.082715877136863902, -0.07147133206917800907 ) ) ;
#6653 = CARTESIAN_POINT ( 'NONE',  ( 54.72065718078918906, 60.70051614449766930, -6.458785618021089192 ) ) ;
#6654 = EDGE_CURVE ( 'NONE', #9272, #11951, #11560, .T. ) ;
#6655 = ORIENTED_EDGE ( 'NONE', *, *, #6545, .F. ) ;
#6656 = ORIENTED_EDGE ( 'NONE', *, *, #11921, .F. ) ;
#6657 = ORIENTED_EDGE ( 'NONE', *, *, #8224, .F. ) ;
#6658 = VERTEX_POINT ( 'NONE', #3115 ) ;
#6659 = CARTESIAN_POINT ( 'NONE',  ( -4.000000000000000000, -2.309401076758515803, -0.4999999999999995559 ) ) ;
#6660 = CARTESIAN_POINT ( 'NONE',  ( -62.49999999999997158, 20.00000000000001421, -9.999999999999998224 ) ) ;
#6661 = CARTESIAN_POINT ( 'NONE',  ( 7.500000000000107470, -32.99038105676652322, -9.000000000000000000 ) ) ;
#6662 = CARTESIAN_POINT ( 'NONE',  ( 51.92680522751233951, 55.59948385550240602, -6.007379884777223289 ) ) ;
#6663 = DIRECTION ( 'NONE',  ( -1.000000000000000000, 0.000000000000000000, -0.000000000000000000 ) ) ;
#6664 = CARTESIAN_POINT ( 'NONE',  ( 43.20883090819742023, 54.20051614449766220, -4.963592699178938972 ) ) ;
#6665 = AXIS2_PLACEMENT_3D ( 'NONE', #8628, #4277, #11544 ) ;
#6666 = DIRECTION ( 'NONE',  ( 4.082155997157843695E-16, -1.000000000000000000, 0.000000000000000000 ) ) ;
#6667 = DIRECTION ( 'NONE',  ( -1.000000000000000000, 0.000000000000000000, 0.000000000000000000 ) ) ;
#6668 = CARTESIAN_POINT ( 'NONE',  ( 52.25172492374527877, 63.40051614449765793, 7.007379884777203749 ) ) ;
#6669 = VERTEX_POINT ( 'NONE', #6629 ) ;
#6670 = DIRECTION ( 'NONE',  ( -0.000000000000000000, -0.000000000000000000, -1.000000000000000000 ) ) ;
#6671 = ORIENTED_EDGE ( 'NONE', *, *, #13165, .F. ) ;
#6672 = CARTESIAN_POINT ( 'NONE',  ( 0.1739375980333722760, 3.358985280702821097, 4.182066831946702479 ) ) ;
#6673 = CIRCLE ( 'NONE', #13270, 15.00000000000000000 ) ;
#6674 = AXIS2_PLACEMENT_3D ( 'NONE', #5628, #10794, #6666 ) ;
#6675 = DIRECTION ( 'NONE',  ( 0.000000000000000000, 0.000000000000000000, 1.000000000000000000 ) ) ;
#6676 = EDGE_CURVE ( 'NONE', #13379, #9523, #13611, .T. ) ;
#6677 = CARTESIAN_POINT ( 'NONE',  ( 4.158921614371310582, -4.076055977742308656, 0.05993604794450350243 ) ) ;
#6678 = APPLICATION_PROTOCOL_DEFINITION ( 'draft international standard', 'automotive_design', 1998, #9727 ) ;
#6679 = CARTESIAN_POINT ( 'NONE',  ( 52.25172492374522903, 57.59948385550241312, -7.007379884777225953 ) ) ;
#6680 = CARTESIAN_POINT ( 'NONE',  ( 4.200000000000001954, 0.000000000000000000, 0.000000000000000000 ) ) ;
#6681 = CARTESIAN_POINT ( 'NONE',  ( 55.08986747509849380, 59.20051614449766220, 3.727524721679155384 ) ) ;
#6682 = CARTESIAN_POINT ( 'NONE',  ( 0.000000000000000000, 0.000000000000000000, -0.3080913168122742518 ) ) ;
#6683 = CARTESIAN_POINT ( 'NONE',  ( 6.445127866599366762, 5.657054305385774917, 0.4229901806197435277 ) ) ;
#6684 = DIRECTION ( 'NONE',  ( 0.000000000000000000, 0.000000000000000000, 1.000000000000000000 ) ) ;
#6685 = CARTESIAN_POINT ( 'NONE',  ( 42.63976443033212860, 64.99948385550240459, 0.02388180880522514787 ) ) ;
#6686 = VECTOR ( 'NONE', #5210, 1000.000000000000000 ) ;
#6687 = DIRECTION ( 'NONE',  ( 1.000000000000000000, 0.000000000000000000, 0.000000000000000000 ) ) ;
#6688 = ORIENTED_EDGE ( 'NONE', *, *, #10596, .T. ) ;
#6689 = ORIENTED_EDGE ( 'NONE', *, *, #9143, .F. ) ;
#6690 = AXIS2_PLACEMENT_3D ( 'NONE', #4314, #6406, #9838 ) ;
#6691 = ORIENTED_EDGE ( 'NONE', *, *, #5013, .T. ) ;
#6692 = DIRECTION ( 'NONE',  ( -0.000000000000000000, -0.000000000000000000, -1.000000000000000000 ) ) ;
#6693 = DIRECTION ( 'NONE',  ( -0.5000000000000041078, 0.8660254037844362651, 0.000000000000000000 ) ) ;
#6694 = DIRECTION ( 'NONE',  ( -1.000000000000000000, 0.000000000000000000, -0.000000000000000000 ) ) ;
#6695 = CARTESIAN_POINT ( 'NONE',  ( 6.245824673232988289, 3.903127342724162840, 3.450227696316072734 ) ) ;
#6696 = CARTESIAN_POINT ( 'NONE',  ( -1.250000000000000000, -6.429618962271402616, -1.000000000000000000 ) ) ;
#6697 = EDGE_CURVE ( 'NONE', #7288, #5220, #1801, .T. ) ;
#6698 = AXIS2_PLACEMENT_3D ( 'NONE', #13392, #2903, #11190 ) ;
#6699 = CARTESIAN_POINT ( 'NONE',  ( 56.65037692655921120, 51.10051614449766078, 2.184720259617097593 ) ) ;
#6700 = ADVANCED_FACE ( 'NONE', ( #3507 ), #6260, .F. ) ;
#6701 = DIRECTION ( 'NONE',  ( 0.03086419753086420623, -0.9995235871707959241, 0.000000000000000000 ) ) ;
#6702 = CARTESIAN_POINT ( 'NONE',  ( 56.65037692655918988, 49.89948385550240317, -2.184720259617163762 ) ) ;
#6703 = CARTESIAN_POINT ( 'NONE',  ( 56.65037692655918988, 45.89948385550240317, -2.184720259617163762 ) ) ;
#6704 = CIRCLE ( 'NONE', #334, 0.4999999999999972244 ) ;
#6705 = CARTESIAN_POINT ( 'NONE',  ( 54.72065718078924590, 64.29948385550240175, 6.458785618021043895 ) ) ;
#6706 = ORIENTED_EDGE ( 'NONE', *, *, #4090, .F. ) ;
#6707 = EDGE_LOOP ( 'NONE', ( #7341, #9359, #3014, #6788 ) ) ;
#6708 = DIRECTION ( 'NONE',  ( 1.000000000000000000, -0.000000000000000000, 0.000000000000000000 ) ) ;
#6709 = ORIENTED_EDGE ( 'NONE', *, *, #1511, .F. ) ;
#6710 = CARTESIAN_POINT ( 'NONE',  ( 4.630153689607048761, 0.000000000000000000, 0.000000000000000000 ) ) ;
#6711 = DIRECTION ( 'NONE',  ( 0.000000000000000000, -0.000000000000000000, 1.000000000000000000 ) ) ;
#6712 = CARTESIAN_POINT ( 'NONE',  ( 51.97223112728249816, 56.60051614449765367, -5.992620115222793586 ) ) ;
#6713 = EDGE_CURVE ( 'NONE', #966, #13576, #953, .T. ) ;
#6714 = DIRECTION ( 'NONE',  ( -0.5000000000000041078, 0.8660254037844362651, 0.000000000000000000 ) ) ;
#6715 = CARTESIAN_POINT ( 'NONE',  ( 54.68390685589033495, 55.69948385550240744, -6.485486291978119766 ) ) ;
#6716 = ADVANCED_FACE ( 'NONE', ( #12514 ), #2135, .F. ) ;
#6717 = CARTESIAN_POINT ( 'NONE',  ( 57.36023556966787851, 55.99948385550239038, -0.02388180880522424582 ) ) ;
#6718 = DIRECTION ( 'NONE',  ( 0.000000000000000000, -0.5000000000000012212, -0.8660254037844380415 ) ) ;
#6719 = AXIS2_PLACEMENT_3D ( 'NONE', #10203, #3085, #8137 ) ;
#6720 = CARTESIAN_POINT ( 'NONE',  ( 45.31609314410960820, 60.30051614449767072, -6.485486291978072693 ) ) ;
#6721 = ORIENTED_EDGE ( 'NONE', *, *, #5950, .T. ) ;
#6722 = ORIENTED_EDGE ( 'NONE', *, *, #11342, .F. ) ;
#6723 = ORIENTED_EDGE ( 'NONE', *, *, #9122, .T. ) ;
#6724 = ORIENTED_EDGE ( 'NONE', *, *, #5560, .F. ) ;
#6725 = DIRECTION ( 'NONE',  ( -0.000000000000000000, -0.000000000000000000, -1.000000000000000000 ) ) ;
#6726 = CIRCLE ( 'NONE', #2741, 15.00000000000000000 ) ;
#6727 = DIRECTION ( 'NONE',  ( -1.000000000000000000, 0.000000000000000000, 0.000000000000000000 ) ) ;
#6728 = CARTESIAN_POINT ( 'NONE',  ( -2.000000000000007550, -3.464101615137749945, 0.000000000000000000 ) ) ;
#6729 = CARTESIAN_POINT ( 'NONE',  ( 53.54508667620428497, 58.29948385550240886, 4.840751629271157874 ) ) ;
#6730 = CARTESIAN_POINT ( 'NONE',  ( 2.385244779468109755E-15, -20.00000000000000000, -9.999999999999994671 ) ) ;
#6731 = CARTESIAN_POINT ( 'NONE',  ( 45.27934281921082516, 51.70051614449765509, 6.458785618021089192 ) ) ;
#6732 = DIRECTION ( 'NONE',  ( -1.000000000000000000, -0.000000000000000000, -0.000000000000000000 ) ) ;
#6733 = DIRECTION ( 'NONE',  ( -0.000000000000000000, 1.000000000000000000, -0.000000000000000000 ) ) ;
#6734 = TOROIDAL_SURFACE ( 'NONE', #12027, 5.200000000000001066, 0.4999999999999978351 ) ;
#6735 = CARTESIAN_POINT ( 'NONE',  ( 49.97728705011495265, 45.50051614449766646, 8.000000000000001776 ) ) ;
#6736 = AXIS2_PLACEMENT_3D ( 'NONE', #5257, #8429, #10220 ) ;
#6737 = ORIENTED_EDGE ( 'NONE', *, *, #7704, .F. ) ;
#6738 = CARTESIAN_POINT ( 'NONE',  ( -1.498123826657861368, -34.92499999999999716, 0.000000000000000000 ) ) ;
#6739 = EDGE_LOOP ( 'NONE', ( #6363, #9153, #4639, #11321, #2003 ) ) ;
#6740 = DIRECTION ( 'NONE',  ( 0.000000000000000000, 0.000000000000000000, -1.000000000000000000 ) ) ;
#6741 = DIRECTION ( 'NONE',  ( -1.000000000000000000, 0.000000000000000000, 0.000000000000000000 ) ) ;
#6742 = DIRECTION ( 'NONE',  ( 0.000000000000000000, 1.000000000000000000, 0.000000000000000000 ) ) ;
#6743 = DIRECTION ( 'NONE',  ( 6.123233995736766036E-17, 0.000000000000000000, 1.000000000000000000 ) ) ;
#6744 = CARTESIAN_POINT ( 'NONE',  ( 42.63976443033212860, 58.99948385550239038, 0.02388180880522514787 ) ) ;
#6745 = VECTOR ( 'NONE', #11591, 1000.000000000000114 ) ;
#6746 = CARTESIAN_POINT ( 'NONE',  ( 44.30067958973594955, 60.10051614449766788, -1.875703265242155693 ) ) ;
#6747 = CARTESIAN_POINT ( 'NONE',  ( 0.000000000000000000, 0.5192545390863916310, 0.000000000000000000 ) ) ;
#6748 = FACE_OUTER_BOUND ( 'NONE', #1209, .T. ) ;
#6749 = CARTESIAN_POINT ( 'NONE',  ( 44.88205777487401349, 63.80051614449766362, 3.688883143319584779 ) ) ;
#6750 = CARTESIAN_POINT ( 'NONE',  ( 46.49166364869460466, 46.69948385550240744, 4.867452303228209765 ) ) ;
#6751 = DIRECTION ( 'NONE',  ( -1.000000000000000000, -0.000000000000000000, -0.000000000000000000 ) ) ;
#6752 = ORIENTED_EDGE ( 'NONE', *, *, #2758, .T. ) ;
#6753 = EDGE_CURVE ( 'NONE', #12170, #504, #692, .T. ) ;
#6754 = VERTEX_POINT ( 'NONE', #319 ) ;
#6755 = DIRECTION ( 'NONE',  ( -1.000000000000000000, -0.000000000000000000, 0.000000000000000000 ) ) ;
#6756 = PRODUCT_RELATED_PRODUCT_CATEGORY ( 'part', '', ( #3662 ) ) ;
#6757 = DIRECTION ( 'NONE',  ( -0.2439756946365075896, 0.9697813467099857254, 1.610118993450814692E-22 ) ) ;
#6758 = CARTESIAN_POINT ( 'NONE',  ( -9.999999999999998224, 15.00000000000001776, -15.00000000000000000 ) ) ;
#6759 = FILL_AREA_STYLE_COLOUR ( '', #4628 ) ;
#6760 = CARTESIAN_POINT ( 'NONE',  ( 6.204460410672266946, 4.828986228461177532, 1.635950503255240607 ) ) ;
#6761 = CARTESIAN_POINT ( 'NONE',  ( -20.00000000000000000, -19.99999999999999289, -23.00000000000000000 ) ) ;
#6762 = CARTESIAN_POINT ( 'NONE',  ( 44.03140696652198471, 55.80051614449766362, 4.306917132069485454 ) ) ;
#6763 = CYLINDRICAL_SURFACE ( 'NONE', #13229, 4.800000000000000711 ) ;
#6764 = CARTESIAN_POINT ( 'NONE',  ( 55.94051828345050836, 51.79948385550240175, -4.345558710429104465 ) ) ;
#6765 = CARTESIAN_POINT ( 'NONE',  ( 55.94051828345050836, 47.79948385550240886, -4.345558710429104465 ) ) ;
#6766 = CIRCLE ( 'NONE', #3236, 8.099999999999999645 ) ;
#6767 = CARTESIAN_POINT ( 'NONE',  ( 45.31609314410967926, 64.69948385550240744, 6.485486291978119766 ) ) ;
#6768 = ORIENTED_EDGE ( 'NONE', *, *, #12852, .F. ) ;
#6769 = EDGE_LOOP ( 'NONE', ( #4166, #6441 ) ) ;
#6770 = DIRECTION ( 'NONE',  ( 0.000000000000000000, 0.000000000000000000, -1.000000000000000000 ) ) ;
#6771 = ORIENTED_EDGE ( 'NONE', *, *, #4791, .F. ) ;
#6772 = CARTESIAN_POINT ( 'NONE',  ( -59.84999999999998721, 32.50000000000001421, 15.00000000000000000 ) ) ;
#6773 = ADVANCED_FACE ( 'NONE', ( #2006 ), #7276, .F. ) ;
#6774 = LINE ( 'NONE', #7748, #3995 ) ;
#6775 = VECTOR ( 'NONE', #6321, 1000.000000000000114 ) ;
#6776 = CARTESIAN_POINT ( 'NONE',  ( 44.28664221472221385, 53.90051614449765793, 1.832500667257213722 ) ) ;
#6777 = CARTESIAN_POINT ( 'NONE',  ( 0.1999999999999987899, 4.286263797015736595E-16, -3.500000000000000000 ) ) ;
#6778 = CARTESIAN_POINT ( 'NONE',  ( 50.02271294988513972, 52.49948385550241170, 8.000000000000001776 ) ) ;
#6779 = CARTESIAN_POINT ( 'NONE',  ( 45.90387839640214196, 56.69948385550240744, 5.676469297603166098 ) ) ;
#6780 = CARTESIAN_POINT ( 'NONE',  ( 4.132952817037861770, -4.063368025374527015, 6.968404583626299416E-17 ) ) ;
#6781 = EDGE_CURVE ( 'NONE', #12922, #7376, #6319, .T. ) ;
#6782 = CARTESIAN_POINT ( 'NONE',  ( 42.38452918213190657, 59.90051614449767214, 2.450534656007115508 ) ) ;
#6783 = ORIENTED_EDGE ( 'NONE', *, *, #4008, .F. ) ;
#6784 = ADVANCED_FACE ( 'NONE', ( #7414 ), #4025, .F. ) ;
#6785 = CONTEXT_DEPENDENT_SHAPE_REPRESENTATION ( #6, #5568 ) ;
#6786 = ORIENTED_EDGE ( 'NONE', *, *, #4684, .F. ) ;
#6787 = EDGE_CURVE ( 'NONE', #11251, #9307, #9972, .T. ) ;
#6788 = ORIENTED_EDGE ( 'NONE', *, *, #3685, .F. ) ;
#6789 = ORIENTED_EDGE ( 'NONE', *, *, #6574, .F. ) ;
#6790 = CARTESIAN_POINT ( 'NONE',  ( 6.244889965166093404, 4.918546365148221078, -1.691415889817839302 ) ) ;
#6791 = SURFACE_STYLE_USAGE ( .BOTH. , #2562 ) ;
#6792 = DIRECTION ( 'NONE',  ( 0.000000000000000000, 0.000000000000000000, 1.000000000000000000 ) ) ;
#6793 = CARTESIAN_POINT ( 'NONE',  ( 2.449293598294706513E-15, -20.00000000000000000, 9.000000000000000000 ) ) ;
#6794 = CARTESIAN_POINT ( 'NONE',  ( 51.97223112728254790, 54.39948385550241028, 5.992620115222778487 ) ) ;
#6795 = CARTESIAN_POINT ( 'NONE',  ( 30.00000000000000000, 1.040834085586084888E-14, 0.000000000000000000 ) ) ;
#6796 = CARTESIAN_POINT ( 'NONE',  ( 49.97728705011495265, 53.50051614449767357, 8.000000000000001776 ) ) ;
#6797 = DIRECTION ( 'NONE',  ( -1.000000000000000000, 0.000000000000000000, 0.000000000000000000 ) ) ;
#6798 = CARTESIAN_POINT ( 'NONE',  ( 51.51576781266200555, 45.00000000000000711, -6.337576802645323859 ) ) ;
#6799 = CARTESIAN_POINT ( 'NONE',  ( 47.74827507625469281, 62.40051614449766504, -7.007379884777203749 ) ) ;
#6800 = VERTEX_POINT ( 'NONE', #1084 ) ;
#6801 = DIRECTION ( 'NONE',  ( 0.000000000000000000, -0.4999999999999991118, 0.8660254037844391517 ) ) ;
#6802 = ORIENTED_EDGE ( 'NONE', *, *, #687, .F. ) ;
#6803 = DIRECTION ( 'NONE',  ( 9.858538378746663627E-23, -5.031452844637890958E-23, 1.000000000000000000 ) ) ;
#6804 = CARTESIAN_POINT ( 'NONE',  ( 3.974175853610014908, -2.726149789692841274, -2.409821656223155806 ) ) ;
#6805 = DIRECTION ( 'NONE',  ( 0.9237280213470682178, 0.3830490080632377725, 0.000000000000000000 ) ) ;
#6806 = CARTESIAN_POINT ( 'NONE',  ( 49.97728705011488159, 55.49948385550240459, -7.000000000000000888 ) ) ;
#6807 = CIRCLE ( 'NONE', #12104, 5.000000000000000000 ) ;
#6808 = ADVANCED_FACE ( 'NONE', ( #12584 ), #10375, .T. ) ;
#6809 = CARTESIAN_POINT ( 'NONE',  ( 55.08986747509849380, 61.20051614449766220, 3.727524721679155384 ) ) ;
#6810 = DIRECTION ( 'NONE',  ( 1.000000000000000000, 0.000000000000000000, 0.000000000000000000 ) ) ;
#6811 = CARTESIAN_POINT ( 'NONE',  ( 2.449293598294706513E-15, -20.00000000000000000, 9.000000000000000000 ) ) ;
#6812 = CARTESIAN_POINT ( 'NONE',  ( 50.02271294988505446, 44.50051614449765935, -7.000000000000000888 ) ) ;
#6813 = CARTESIAN_POINT ( 'NONE',  ( 44.30067958973596376, 48.89948385550241028, 1.875703265242204099 ) ) ;
#6814 = DIRECTION ( 'NONE',  ( -1.000000000000000000, 1.734723475976807094E-16, 0.000000000000000000 ) ) ;
#6815 = ORIENTED_EDGE ( 'NONE', *, *, #8305, .F. ) ;
#6816 = AXIS2_PLACEMENT_3D ( 'NONE', #6016, #6300, #12495 ) ;
#6817 = EDGE_LOOP ( 'NONE', ( #12338, #10351, #10371, #9100 ) ) ;
#6818 = CARTESIAN_POINT ( 'NONE',  ( -6.165086708099547508, -6.325508935188330462, -9.000000000000000000 ) ) ;
#6819 = PRESENTATION_LAYER_ASSIGNMENT (  '', '', ( #10567 ) ) ;
#6820 = CARTESIAN_POINT ( 'NONE',  ( -62.49999999999997158, 32.50000000000001421, 9.999999999999998224 ) ) ;
#6821 = DIRECTION ( 'NONE',  ( 0.1836763462126260738, -0.9829867750086873635, -1.521953536530129477E-22 ) ) ;
#6822 = CARTESIAN_POINT ( 'NONE',  ( 2.000000000000000000, 0.8865213383406680414, -1.535500000000000975 ) ) ;
#6823 = CARTESIAN_POINT ( 'NONE',  ( 0.000000000000000000, 0.000000000000000000, -4.974599999999998801 ) ) ;
#6824 = CARTESIAN_POINT ( 'NONE',  ( 43.34962307344078880, 62.10051614449766078, -2.184720259617096705 ) ) ;
#6825 = AXIS2_PLACEMENT_3D ( 'NONE', #781, #1828, #1899 ) ;
#6826 = CARTESIAN_POINT ( 'NONE',  ( 6.390983168987730778, -3.014662706507984513, -5.000000000000000000 ) ) ;
#6827 = DIRECTION ( 'NONE',  ( -0.000000000000000000, -0.000000000000000000, 1.000000000000000000 ) ) ;
#6828 = CARTESIAN_POINT ( 'NONE',  ( 55.94051828345050836, 53.79948385550238754, -4.345558710429104465 ) ) ;
#6829 = CARTESIAN_POINT ( 'NONE',  ( 47.74827507625478518, 48.59948385550239180, 7.007379884777227730 ) ) ;
#6830 = AXIS2_PLACEMENT_3D ( 'NONE', #2435, #362, #4589 ) ;
#6831 = CARTESIAN_POINT ( 'NONE',  ( 45.31609314410967926, 60.69948385550240033, 6.485486291978119766 ) ) ;
#6832 = ORIENTED_EDGE ( 'NONE', *, *, #3459, .T. ) ;
#6833 = VERTEX_POINT ( 'NONE', #6381 ) ;
#6834 = DIRECTION ( 'NONE',  ( -4.082155997157844188E-16, 1.000000000000000000, 0.000000000000000000 ) ) ;
#6835 = AXIS2_PLACEMENT_3D ( 'NONE', #5813, #5879, #3720 ) ;
#6836 = ORIENTED_EDGE ( 'NONE', *, *, #849, .F. ) ;
#6837 = DIRECTION ( 'NONE',  ( 1.000000000000000000, 0.000000000000000000, 0.000000000000000000 ) ) ;
#6838 = CARTESIAN_POINT ( 'NONE',  ( 1.925929944387235853E-31, 15.00000000000001599, 15.00000000000000178 ) ) ;
#6839 = CARTESIAN_POINT ( 'NONE',  ( 44.28664221472221385, 51.90051614449765793, 1.832500667257213722 ) ) ;
#6840 = CARTESIAN_POINT ( 'NONE',  ( 4.000000000000000000, -1.677850389431204459, -3.535268758346977513 ) ) ;
#6841 = PRODUCT_DEFINITION_FORMATION_WITH_SPECIFIED_SOURCE ( 'ANY', '', #3464, .NOT_KNOWN. ) ;
#6842 = CARTESIAN_POINT ( 'NONE',  ( 47.37792948025162332, 53.39948385550241028, -7.992620115222770494 ) ) ;
#6843 = CIRCLE ( 'NONE', #7742, 1.999999999999998224 ) ;
#6844 = CARTESIAN_POINT ( 'NONE',  ( 42.63976443033212860, 58.99948385550239038, 0.02388180880522514787 ) ) ;
#6845 = CARTESIAN_POINT ( 'NONE',  ( 4.630153689607048761, 0.000000000000000000, 0.000000000000000000 ) ) ;
#6846 = EDGE_CURVE ( 'NONE', #13409, #10472, #7561, .T. ) ;
#6847 = CARTESIAN_POINT ( 'NONE',  ( 58.41169779390614281, 61.00051614449765935, 0.02388180880515032231 ) ) ;
#6848 = EDGE_LOOP ( 'NONE', ( #8326, #7827, #10216, #4626 ) ) ;
#6849 = ITEM_DEFINED_TRANSFORMATION ( 'NONE', 'NONE', #13216,  #430 ) ;
#6850 = ORIENTED_EDGE ( 'NONE', *, *, #7882, .T. ) ;
#6851 = ORIENTED_EDGE ( 'NONE', *, *, #9890, .F. ) ;
#6852 = ORIENTED_EDGE ( 'NONE', *, *, #11322, .F. ) ;
#6853 = CARTESIAN_POINT ( 'NONE',  ( 20.00000000000000000, -25.00000000000000711, -23.00000000000000000 ) ) ;
#6854 = CIRCLE ( 'NONE', #877, 4.000000000000003553 ) ;
#6855 = ADVANCED_FACE ( 'NONE', ( #3441 ), #4546, .T. ) ;
#6856 = DIRECTION ( 'NONE',  ( -0.000000000000000000, 0.000000000000000000, -1.000000000000000000 ) ) ;
#6857 = LINE ( 'NONE', #11061, #10303 ) ;
#6858 = CARTESIAN_POINT ( 'NONE',  ( 50.02271294988511841, 58.49948385550241170, 6.000000000000000888 ) ) ;
#6859 = CARTESIAN_POINT ( 'NONE',  ( 55.96859303347802239, 48.80051614449765651, -4.306917132069484566 ) ) ;
#6860 = ADVANCED_FACE ( 'NONE', ( #6179 ), #887, .F. ) ;
#6861 = CARTESIAN_POINT ( 'NONE',  ( 56.81924384183006538, 52.80051614449766362, -4.924951120819380357 ) ) ;
#6862 = EDGE_CURVE ( 'NONE', #11927, #7440, #9926, .T. ) ;
#6863 = DIRECTION ( 'NONE',  ( -0.000000000000000000, -0.000000000000000000, 1.000000000000000000 ) ) ;
#6864 = LINE ( 'NONE', #9003, #4701 ) ;
#6865 = CARTESIAN_POINT ( 'NONE',  ( 45.90387839640208512, 62.30051614449766362, -5.676469297603124353 ) ) ;
#6866 = CIRCLE ( 'NONE', #885, 1.999999999999998224 ) ;
#6867 = ORIENTED_EDGE ( 'NONE', *, *, #1036, .T. ) ;
#6868 = CYLINDRICAL_SURFACE ( 'NONE', #4861, 6.080745460913608902 ) ;
#6869 = ORIENTED_EDGE ( 'NONE', *, *, #3560, .T. ) ;
#6870 = DIRECTION ( 'NONE',  ( -1.000000000000000000, 0.000000000000000000, 0.000000000000000000 ) ) ;
#6871 = DIRECTION ( 'NONE',  ( 0.000000000000000000, 0.000000000000000000, 1.000000000000000000 ) ) ;
#6872 = AXIS2_PLACEMENT_3D ( 'NONE', #11801, #13659, #1144 ) ;
#6873 = DIRECTION ( 'NONE',  ( 0.5135024480563477045, 0.000000000000000000, 0.8580881282479897454 ) ) ;
#6874 = CARTESIAN_POINT ( 'NONE',  ( 56.66441430157296821, 56.09948385550240602, 2.141517661632100111 ) ) ;
#6875 = CARTESIAN_POINT ( 'NONE',  ( 56.66441430157296821, 50.09948385550240602, 2.141517661632100111 ) ) ;
#6876 = CARTESIAN_POINT ( 'NONE',  ( 48.02776887271750184, 59.60051614449765367, 5.992620115222795363 ) ) ;
#6877 = CARTESIAN_POINT ( 'NONE',  ( 8.500000000000000000, -2.886751345948119774, 4.999999999999999112 ) ) ;
#6878 = DIRECTION ( 'NONE',  ( 0.000000000000000000, 0.000000000000000000, 1.000000000000000000 ) ) ;
#6879 = CARTESIAN_POINT ( 'NONE',  ( 52.29715082351538769, 46.60051614449766078, -6.992620115222796251 ) ) ;
#6880 = CARTESIAN_POINT ( 'NONE',  ( 44.03140696652192787, 65.19948385550240744, -4.306917132069425058 ) ) ;
#6881 = DIRECTION ( 'NONE',  ( 0.000000000000000000, 0.000000000000000000, 1.000000000000000000 ) ) ;
#6882 = EDGE_LOOP ( 'NONE', ( #5119, #5369, #7456, #473, #2786 ) ) ;
#6883 = CIRCLE ( 'NONE', #13046, 5.000000000000000888 ) ;
#6884 = VECTOR ( 'NONE', #12575, 1000.000000000000000 ) ;
#6885 = PRODUCT_DEFINITION_CONTEXT ( 'detailed design', #9203, 'design' ) ;
#6886 = CONICAL_SURFACE ( 'NONE', #9099, 3.500000000000000000, 1.047197551196600296 ) ;
#6887 = ORIENTED_EDGE ( 'NONE', *, *, #11081, .F. ) ;
#6888 = ORIENTED_EDGE ( 'NONE', *, *, #7727, .F. ) ;
#6889 = CYLINDRICAL_SURFACE ( 'NONE', #9251, 5.000000000000000888 ) ;
#6890 = CARTESIAN_POINT ( 'NONE',  ( 4.141042297810615835, -2.227970268150433863, -3.687027686973623819 ) ) ;
#6891 =( BOUNDED_SURFACE ( )  B_SPLINE_SURFACE ( 3, 2, ( 
 ( #7355, #11566, #13617 ),
 ( #10241, #12314, #4027 ),
 ( #7145, #755, #12521 ),
 ( #13405, #11494, #818 ),
 ( #2991, #7214, #12451 ),
 ( #2077, #6326, #6261 ) ),
 .UNSPECIFIED., .F., .F., .F. ) 
 B_SPLINE_SURFACE_WITH_KNOTS ( ( 4, 2, 4 ),
 ( 3, 3 ),
 ( 0.02027752710269158445, 0.02273781595091097299, 0.02519810479913036153 ),
 ( 0.000000000000000000, 1.000000000000000000 ),
 .UNSPECIFIED. ) 
 GEOMETRIC_REPRESENTATION_ITEM ( )  RATIONAL_B_SPLINE_SURFACE ( (
 ( 1.000000000000000000, 0.8047781431712808242, 1.000000000000000000),
 ( 1.000000000000000000, 0.8123773247083928561, 1.000000000000000000),
 ( 1.000000000000000000, 0.8190670192154906326, 1.000000000000000000),
 ( 1.000000000000000000, 0.8192353552912178261, 1.000000000000000000),
 ( 1.000000000000000000, 0.8126132098226825917, 1.000000000000000000),
 ( 1.000000000000000000, 0.8047712465856394770, 1.000000000000000000) ) ) 
 REPRESENTATION_ITEM ( '' )  SURFACE ( )  );
#6892 = DIRECTION ( 'NONE',  ( -0.000000000000000000, -1.000000000000000000, -0.000000000000000000 ) ) ;
#6893 = LINE ( 'NONE', #7800, #7129 ) ;
#6894 = LINE ( 'NONE', #11101, #683 ) ;
#6895 = EDGE_CURVE ( 'NONE', #11319, #5687, #6893, .T. ) ;
#6896 = VECTOR ( 'NONE', #25, 1000.000000000000000 ) ;
#6897 = CARTESIAN_POINT ( 'NONE',  ( 49.97728705011495265, 57.50051614449766646, 7.000000000000000888 ) ) ;
#6898 = CARTESIAN_POINT ( 'NONE',  ( 0.1973348417602843741, -1.936114729415326696, -5.000000000000000000 ) ) ;
#6899 = AXIS2_PLACEMENT_3D ( 'NONE', #7497, #6469, #5433 ) ;
#6900 = LINE ( 'NONE', #2745, #12899 ) ;
#6901 = CARTESIAN_POINT ( 'NONE',  ( 49.97728705011488159, 57.49948385550241170, -7.000000000000000888 ) ) ;
#6902 = CARTESIAN_POINT ( 'NONE',  ( 42.63976443033212860, 48.99948385550240459, 0.02388180880522514787 ) ) ;
#6903 = CARTESIAN_POINT ( 'NONE',  ( 56.66441430157296821, 46.09948385550240602, 2.141517661632100111 ) ) ;
#6904 = VERTEX_POINT ( 'NONE', #8905 ) ;
#6905 = VERTEX_POINT ( 'NONE', #13301 ) ;
#6906 = CARTESIAN_POINT ( 'NONE',  ( 0.1999999999999987899, 0.000000000000000000, 0.000000000000000000 ) ) ;
#6907 = ORIENTED_EDGE ( 'NONE', *, *, #3563, .F. ) ;
#6908 = PLANE ( 'NONE',  #9163 ) ;
#6909 = AXIS2_PLACEMENT_3D ( 'NONE', #9681, #1030, #12848 ) ;
#6910 = CARTESIAN_POINT ( 'NONE',  ( 6.367873360227558344, -2.886751345948133984, -5.000000000000000000 ) ) ;
#6911 = CARTESIAN_POINT ( 'NONE',  ( 48.07319477248762496, 62.40051614449765793, -6.007379884777208190 ) ) ;
#6912 = AXIS2_PLACEMENT_3D ( 'NONE', #11571, #4234, #6125 ) ;
#6913 = CARTESIAN_POINT ( 'NONE',  ( 0.000000000000000000, 0.000000000000000000, -3.499999999999999556 ) ) ;
#6914 = CARTESIAN_POINT ( 'NONE',  ( 52.57664461997811856, 57.59948385550240602, -8.007379884777229506 ) ) ;
#6915 = CARTESIAN_POINT ( 'NONE',  ( 43.33558569842703179, 65.09948385550239891, -2.141517661632099223 ) ) ;
#6916 = CARTESIAN_POINT ( 'NONE',  ( 6.367873360227556567, 2.886751345948123770, -5.000000000000000000 ) ) ;
#6917 = CARTESIAN_POINT ( 'NONE',  ( 56.81924384183006538, 62.80051614449766362, -4.924951120819380357 ) ) ;
#6918 = ORIENTED_EDGE ( 'NONE', *, *, #9413, .F. ) ;
#6919 = EDGE_LOOP ( 'NONE', ( #12204, #11480, #2016, #722 ) ) ;
#6920 = ORIENTED_EDGE ( 'NONE', *, *, #497, .F. ) ;
#6921 = EDGE_CURVE ( 'NONE', #2018, #4052, #5370, .T. ) ;
#6922 = EDGE_LOOP ( 'NONE', ( #8065, #13609, #10180, #6014 ) ) ;
#6923 = CARTESIAN_POINT ( 'NONE',  ( -3.309651814758565180, -5.455921364805393026, 0.000000000000000000 ) ) ;
#6924 = EDGE_CURVE ( 'NONE', #10006, #11927, #4615, .T. ) ;
#6925 = LINE ( 'NONE', #9069, #2918 ) ;
#6926 = DIRECTION ( 'NONE',  ( -1.000000000000000000, 0.000000000000000000, 0.000000000000000000 ) ) ;
#6927 = CARTESIAN_POINT ( 'NONE',  ( 13.67449106481173615, -26.16508670809940895, 9.000000000000000000 ) ) ;
#6928 = CARTESIAN_POINT ( 'NONE',  ( 56.30877334542961421, 63.99948385550241170, -0.02388180880520959434 ) ) ;
#6929 = CARTESIAN_POINT ( 'NONE',  ( 44.05948171654945611, 52.20051614449765509, -4.345558710429044069 ) ) ;
#6930 = CARTESIAN_POINT ( 'NONE',  ( 52.62207051974829852, 52.60051614449765367, -7.992620115222797139 ) ) ;
#6931 = DIRECTION ( 'NONE',  ( 0.000000000000000000, 0.000000000000000000, -1.000000000000000000 ) ) ;
#6932 = CARTESIAN_POINT ( 'NONE',  ( -20.00000000000000000, -25.00000000000000000, -23.00000000000000000 ) ) ;
#6933 = B_SPLINE_CURVE_WITH_KNOTS ( 'NONE', 3,
 ( #3354, #12683, #8350, #169, #11651, #1194 ),
 .UNSPECIFIED., .F., .F.,
 ( 4, 2, 4 ),
 ( 0.003358874760055550156, 0.004541967308452096383, 0.005725059856848641743 ),
 .UNSPECIFIED. ) ;
#6934 = CARTESIAN_POINT ( 'NONE',  ( 55.96859303347802239, 62.80051614449766362, -4.306917132069484566 ) ) ;
#6936 = ORIENTED_EDGE ( 'NONE', *, *, #6474, .F. ) ;
#6935 = ORIENTED_EDGE ( 'NONE', *, *, #11542, .T. ) ;
#6937 = DIRECTION ( 'NONE',  ( 1.000000000000000000, 0.000000000000000000, 0.000000000000000000 ) ) ;
#6938 = VECTOR ( 'NONE', #9692, 999.9999999999998863 ) ;
#6939 = EDGE_LOOP ( 'NONE', ( #3028, #3733, #3368, #198 ) ) ;
#6940 = LINE ( 'NONE', #1388, #10699 ) ;
#6941 = AXIS2_PLACEMENT_3D ( 'NONE', #5300, #7165, #6344 ) ;
#6942 = CARTESIAN_POINT ( 'NONE',  ( 2.449293598294706513E-15, -20.00000000000000000, -23.00000000000000000 ) ) ;
#6943 = CARTESIAN_POINT ( 'NONE',  ( 3.851859888774471706E-31, 15.00000000000001599, -20.00000000000000000 ) ) ;
#6944 = CARTESIAN_POINT ( 'NONE',  ( 47.70284917648453415, 59.39948385550241028, -6.992620115222774047 ) ) ;
#6945 = CARTESIAN_POINT ( 'NONE',  ( 47.74827507625477807, 58.59948385550239180, 7.007379884777229506 ) ) ;
#6946 = CIRCLE ( 'NONE', #6308, 2.396904916527699214 ) ;
#6947 = EDGE_CURVE ( 'NONE', #6494, #12390, #8895, .T. ) ;
#6948 = CARTESIAN_POINT ( 'NONE',  ( 7.900000000000002132, 0.000000000000000000, 0.000000000000000000 ) ) ;
#6949 = AXIS2_PLACEMENT_3D ( 'NONE', #2334, #10713, #1289 ) ;
#6950 = DIRECTION ( 'NONE',  ( -1.000000000000000000, -0.000000000000000000, -0.000000000000000000 ) ) ;
#6951 = CARTESIAN_POINT ( 'NONE',  ( -20.00000000000000000, -19.99999999999999289, -23.00000000000000000 ) ) ;
#6952 = CARTESIAN_POINT ( 'NONE',  ( 55.69932041026405045, 63.10051614449766078, 1.875703265242156359 ) ) ;
#6953 = CARTESIAN_POINT ( 'NONE',  ( 53.50833635130540955, 53.69948385550240744, -4.867452303228209765 ) ) ;
#6954 = CARTESIAN_POINT ( 'NONE',  ( 0.000000000000000000, 0.000000000000000000, 0.000000000000000000 ) ) ;
#6955 = ORIENTED_EDGE ( 'NONE', *, *, #6621, .F. ) ;
#6956 = VECTOR ( 'NONE', #12559, 1000.000000000000000 ) ;
#6957 = VERTEX_POINT ( 'NONE', #4752 ) ;
#6959 = EDGE_CURVE ( 'NONE', #5390, #1735, #1547, .T. ) ;
#6958 = ORIENTED_EDGE ( 'NONE', *, *, #10231, .F. ) ;
#6960 = CARTESIAN_POINT ( 'NONE',  ( 1.250000000000000000, -6.429618962271402616, -1.000000000000000000 ) ) ;
#6961 = ADVANCED_FACE ( 'NONE', ( #12076 ), #11733, .F. ) ;
#6962 = CARTESIAN_POINT ( 'NONE',  ( 3.455068668934414777, -2.624017327439094327, -3.316620875263732504 ) ) ;
#6963 = CARTESIAN_POINT ( 'NONE',  ( -0.1481481481481481122, -4.797713218419819903, -1.000000000000000000 ) ) ;
#6964 =( NAMED_UNIT ( * ) SI_UNIT ( $, .STERADIAN. ) SOLID_ANGLE_UNIT ( ) );
#6965 = DIRECTION ( 'NONE',  ( -0.000000000000000000, -0.000000000000000000, 1.000000000000000000 ) ) ;
#6966 = EDGE_CURVE ( 'NONE', #7271, #2590, #639, .T. ) ;
#6967 = CARTESIAN_POINT ( 'NONE',  ( 0.000000000000000000, 0.000000000000000000, 0.000000000000000000 ) ) ;
#6968 = CARTESIAN_POINT ( 'NONE',  ( 44.05948171654945611, 60.20051614449764799, -4.345558710429044069 ) ) ;
#6969 = CARTESIAN_POINT ( 'NONE',  ( 2.649999999999988365, 15.00000000000001599, 9.999999999999998224 ) ) ;
#6970 = CARTESIAN_POINT ( 'NONE',  ( 51.97223112728249816, 46.60051614449764656, -5.992620115222793586 ) ) ;
#6971 = DIRECTION ( 'NONE',  ( -0.000000000000000000, -0.000000000000000000, 1.000000000000000000 ) ) ;
#6972 = CARTESIAN_POINT ( 'NONE',  ( 52.25172492374522903, 55.59948385550241312, -7.007379884777225953 ) ) ;
#6973 = CARTESIAN_POINT ( 'NONE',  ( 57.36023556966787851, 45.99948385550238328, -0.02388180880522424582 ) ) ;
#6974 = CARTESIAN_POINT ( 'NONE',  ( 47.74827507625478518, 48.59948385550239180, 7.007379884777227730 ) ) ;
#6975 = EDGE_LOOP ( 'NONE', ( #12454, #6428, #13326, #13255 ) ) ;
#6976 = VERTEX_POINT ( 'NONE', #381 ) ;
#6977 = CARTESIAN_POINT ( 'NONE',  ( 22.00000000000000000, -20.00000000000000000, -12.00000000000000000 ) ) ;
#6978 = ORIENTED_EDGE ( 'NONE', *, *, #11817, .T. ) ;
#6979 = DIRECTION ( 'NONE',  ( -0.000000000000000000, -0.000000000000000000, -1.000000000000000000 ) ) ;
#6980 = CYLINDRICAL_SURFACE ( 'NONE', #1750, 0.7500000000000000000 ) ;
#6981 = CARTESIAN_POINT ( 'NONE',  ( 49.97728705011494554, 63.50051614449765935, 6.000000000000000888 ) ) ;
#6982 = CARTESIAN_POINT ( 'NONE',  ( 0.000000000000000000, 0.000000000000000000, 0.000000000000000000 ) ) ;
#6983 = CARTESIAN_POINT ( 'NONE',  ( 45.27934281921075410, 61.29948385550240886, -6.458785618021043895 ) ) ;
#6984 = CARTESIAN_POINT ( 'NONE',  ( 0.000000000000000000, 0.5192545390863916310, -1.000000000000000000 ) ) ;
#6985 = DIRECTION ( 'NONE',  ( -1.000000000000000000, -4.082155997157843695E-16, 0.000000000000000000 ) ) ;
#6986 = CARTESIAN_POINT ( 'NONE',  ( 54.68390685589033495, 47.69948385550240744, -6.485486291978119766 ) ) ;
#6987 = VERTEX_POINT ( 'NONE', #4817 ) ;
#6988 = ORIENTED_EDGE ( 'NONE', *, *, #689, .T. ) ;
#6989 = VECTOR ( 'NONE', #11086, 1000.000000000000000 ) ;
#6990 = EDGE_LOOP ( 'NONE', ( #9553, #8439, #8556, #1680 ) ) ;
#6991 = ORIENTED_EDGE ( 'NONE', *, *, #10818, .F. ) ;
#6992 = PLANE ( 'NONE',  #9259 ) ;
#6993 = EDGE_CURVE ( 'NONE', #5480, #4363, #2929, .T. ) ;
#6994 = AXIS2_PLACEMENT_3D ( 'NONE', #4440, #2496, #5553 ) ;
#6995 = FACE_OUTER_BOUND ( 'NONE', #13060, .T. ) ;
#6996 = CARTESIAN_POINT ( 'NONE',  ( 2.500000000000000888, 3.061616997868384127E-16, -4.974599999999998801 ) ) ;
#6997 = DIRECTION ( 'NONE',  ( -1.000000000000000000, 0.000000000000000000, 0.000000000000000000 ) ) ;
#6998 = DIRECTION ( 'NONE',  ( 1.000000000000000000, 3.469446951953615175E-16, 0.000000000000000000 ) ) ;
#6999 = CARTESIAN_POINT ( 'NONE',  ( 49.97728705011488870, 61.49948385550241170, -6.000000000000000888 ) ) ;
#7000 = CARTESIAN_POINT ( 'NONE',  ( 45.86712807150329496, 55.70051614449766220, 5.649768623646139964 ) ) ;
#7001 = CARTESIAN_POINT ( 'NONE',  ( 58.41169779390614281, 61.00051614449765935, 0.02388180880515032231 ) ) ;
#7002 = SURFACE_STYLE_USAGE ( .BOTH. , #609 ) ;
#7003 = DIRECTION ( 'NONE',  ( -0.5000000000000061062, 0.000000000000000000, 0.8660254037844351549 ) ) ;
#7004 = CARTESIAN_POINT ( 'NONE',  ( 57.61547081786810764, 48.90051614449766504, -2.450534656007114176 ) ) ;
#7006 = ORIENTED_EDGE ( 'NONE', *, *, #1265, .T. ) ;
#7005 = ORIENTED_EDGE ( 'NONE', *, *, #2975, .F. ) ;
#7007 = CARTESIAN_POINT ( 'NONE',  ( 1.144235203016666258, 3.958177651039090250, -0.09382832055445661235 ) ) ;
#7008 = ORIENTED_EDGE ( 'NONE', *, *, #9951, .T. ) ;
#7009 = CARTESIAN_POINT ( 'NONE',  ( 2.449293598294706513E-15, -20.00000000000000000, 9.000000000000000000 ) ) ;
#7010 = DIRECTION ( 'NONE',  ( 1.000000000000000000, 0.000000000000000000, 0.000000000000000000 ) ) ;
#7011 = CARTESIAN_POINT ( 'NONE',  ( 44.05948171654949874, 64.79948385550240175, 4.345558710429105354 ) ) ;
#7012 = CARTESIAN_POINT ( 'NONE',  ( 47.74827507625477807, 56.59948385550240602, 7.007379884777229506 ) ) ;
#7013 = CARTESIAN_POINT ( 'NONE',  ( 7.499999999999834799, -7.009618943233325794, 9.000000000000000000 ) ) ;
#7014 = CARTESIAN_POINT ( 'NONE',  ( 2.449293598294706513E-15, -20.00000000000000000, -20.00000000000000000 ) ) ;
#7015 = DIRECTION ( 'NONE',  ( 1.000000000000000000, 0.000000000000000000, 0.000000000000000000 ) ) ;
#7016 = CARTESIAN_POINT ( 'NONE',  ( 49.97728705011494554, 63.50051614449765935, 6.000000000000000888 ) ) ;
#7017 = CARTESIAN_POINT ( 'NONE',  ( 51.92680522751233951, 53.59948385550240602, -6.007379884777223289 ) ) ;
#7018 = CARTESIAN_POINT ( 'NONE',  ( -62.49999999999997158, 45.00000000000001421, 15.00000000000000000 ) ) ;
#7019 = ADVANCED_FACE ( 'NONE', ( #12210 ), #8835, .T. ) ;
#7020 = ORIENTED_EDGE ( 'NONE', *, *, #3988, .F. ) ;
#7021 = ORIENTED_EDGE ( 'NONE', *, *, #13165, .T. ) ;
#7022 = ORIENTED_EDGE ( 'NONE', *, *, #1689, .F. ) ;
#7023 = CARTESIAN_POINT ( 'NONE',  ( 13.99999999999999822, 2.210487472460973684E-16, -1.610000000000000098 ) ) ;
#7024 = PRESENTATION_LAYER_ASSIGNMENT (  '', '', ( #13629 ) ) ;
#7025 = DIRECTION ( 'NONE',  ( -0.000000000000000000, -0.000000000000000000, -1.000000000000000000 ) ) ;
#7026 = DIRECTION ( 'NONE',  ( -0.000000000000000000, -0.000000000000000000, 1.000000000000000000 ) ) ;
#7027 = FILL_AREA_STYLE ('',( #7999 ) ) ;
#7028 = CARTESIAN_POINT ( 'NONE',  ( -19.99999999999999289, -14.99999999999998579, -20.00000000000000000 ) ) ;
#7029 = DIRECTION ( 'NONE',  ( 0.000000000000000000, 0.000000000000000000, 1.000000000000000000 ) ) ;
#7030 = EDGE_CURVE ( 'NONE', #6571, #4657, #3577, .T. ) ;
#7031 = CARTESIAN_POINT ( 'NONE',  ( -14.92499999999998828, -21.49812382665791688, 0.000000000000000000 ) ) ;
#7032 = CARTESIAN_POINT ( 'NONE',  ( 44.30067958973594955, 46.10051614449766078, -1.875703265242155693 ) ) ;
#7033 = EDGE_CURVE ( 'NONE', #5030, #10021, #2527, .T. ) ;
#7034 = CARTESIAN_POINT ( 'NONE',  ( 0.000000000000000000, 0.000000000000000000, 0.000000000000000000 ) ) ;
#7035 = CARTESIAN_POINT ( 'NONE',  ( 54.09612160359786515, 57.69948385550240744, -5.676469297603166098 ) ) ;
#7036 = CARTESIAN_POINT ( 'NONE',  ( 52.25172492374522903, 51.59948385550240602, -7.007379884777225953 ) ) ;
#7037 = ADVANCED_FACE ( 'NONE', ( #1478 ), #5930, .F. ) ;
#7038 = AXIS2_PLACEMENT_3D ( 'NONE', #12006, #6692, #12206 ) ;
#7039 = ORIENTED_EDGE ( 'NONE', *, *, #4901, .T. ) ;
#7040 = CARTESIAN_POINT ( 'NONE',  ( 55.94051828345050836, 49.79948385550240175, -4.345558710429104465 ) ) ;
#7041 = AXIS2_PLACEMENT_3D ( 'NONE', #13108, #13038, #8772 ) ;
#7042 = ORIENTED_EDGE ( 'NONE', *, *, #13109, .F. ) ;
#7043 = EDGE_LOOP ( 'NONE', ( #8028, #12374, #5008, #3218 ) ) ;
#7044 = CARTESIAN_POINT ( 'NONE',  ( -9.999999999999996447, 25.00000000000001776, 15.00000000000000000 ) ) ;
#7045 = EDGE_LOOP ( 'NONE', ( #987, #12807, #3587, #3450, #6390 ) ) ;
#7046 = CARTESIAN_POINT ( 'NONE',  ( 4.170895651974848128, 2.054890354522668439, 3.559174498016340227 ) ) ;
#7047 = AXIS2_PLACEMENT_3D ( 'NONE', #2734, #11166, #5925 ) ;
#7048 = CARTESIAN_POINT ( 'NONE',  ( 3.973514160553462737, 3.435084588004190476, -1.181876024140317227 ) ) ;
#7049 = CARTESIAN_POINT ( 'NONE',  ( 46.49166364869456913, 60.30051614449767072, -4.867452303228181343 ) ) ;
#7050 = CARTESIAN_POINT ( 'NONE',  ( 2.449293598294706513E-15, -20.00000000000000000, -50.00000000000000000 ) ) ;
#7051 = EDGE_CURVE ( 'NONE', #898, #9858, #3138, .T. ) ;
#7052 = CARTESIAN_POINT ( 'NONE',  ( 45.31609314410967926, 58.69948385550240033, 6.485486291978119766 ) ) ;
#7053 = EDGE_CURVE ( 'NONE', #4571, #9009, #2674, .T. ) ;
#7054 = CARTESIAN_POINT ( 'NONE',  ( 2.449293598294706513E-15, -20.00000000000000000, -8.999999999999998224 ) ) ;
#7055 = CARTESIAN_POINT ( 'NONE',  ( 2.449293598294706513E-15, -20.00000000000000000, 9.999999999999998224 ) ) ;
#7056 = CARTESIAN_POINT ( 'NONE',  ( 52.57664461997811856, 51.59948385550240602, -8.007379884777229506 ) ) ;
#7057 = EDGE_LOOP ( 'NONE', ( #8438, #6689, #181, #7412 ) ) ;
#7058 = ORIENTED_EDGE ( 'NONE', *, *, #6697, .F. ) ;
#7059 = ORIENTED_EDGE ( 'NONE', *, *, #2638, .T. ) ;
#7060 = CARTESIAN_POINT ( 'NONE',  ( 2.000000000000000000, 1.773042676681340524, -2.059984127722458425E-15 ) ) ;
#7061 = DIRECTION ( 'NONE',  ( 1.000000000000000000, 0.000000000000000000, 0.000000000000000000 ) ) ;
#7062 =( NAMED_UNIT ( * ) SI_UNIT ( $, .STERADIAN. ) SOLID_ANGLE_UNIT ( ) );
#7063 = DIRECTION ( 'NONE',  ( -1.000000000000000000, 0.000000000000000000, 0.000000000000000000 ) ) ;
#7064 = CARTESIAN_POINT ( 'NONE',  ( 3.951447005078450925, -2.357513599190971032, 2.916666666666666963 ) ) ;
#7065 = PRODUCT_DEFINITION_FORMATION_WITH_SPECIFIED_SOURCE ( 'ANY', '', #443, .NOT_KNOWN. ) ;
#7066 = CARTESIAN_POINT ( 'NONE',  ( -74.99999999999998579, -7.500000000000027534, 10.00000000000000000 ) ) ;
#7067 = CARTESIAN_POINT ( 'NONE',  ( 55.69932041026404335, 61.89948385550241738, -1.875703265242203432 ) ) ;
#7068 = CARTESIAN_POINT ( 'NONE',  ( 50.02271294988505446, 54.50051614449765935, -7.000000000000000888 ) ) ;
#7069 = CARTESIAN_POINT ( 'NONE',  ( 57.60143344285435774, 57.10051614449766788, 2.493737253992045044 ) ) ;
#7070 = EDGE_CURVE ( 'NONE', #5875, #9486, #3123, .T. ) ;
#7071 = ADVANCED_FACE ( 'NONE', ( #8497, #12895 ), #5258, .T. ) ;
#7072 = CARTESIAN_POINT ( 'NONE',  ( 4.071447262713887127, 2.020725942163686284, -3.499999999999999556 ) ) ;
#7073 = CARTESIAN_POINT ( 'NONE',  ( 56.79116909180259398, 53.20051614449766220, 4.963592699178938972 ) ) ;
#7075 = ORIENTED_EDGE ( 'NONE', *, *, #12859, .F. ) ;
#7074 = EDGE_LOOP ( 'NONE', ( #4976, #7151, #7958, #10 ) ) ;
#7076 = VECTOR ( 'NONE', #929, 1000.000000000000000 ) ;
#7077 = CARTESIAN_POINT ( 'NONE',  ( 20.00000000000000000, -14.99999999999999289, -23.00000000000000000 ) ) ;
#7078 = VERTEX_POINT ( 'NONE', #4407 ) ;
#7079 = VERTEX_POINT ( 'NONE', #9528 ) ;
#7080 = CARTESIAN_POINT ( 'NONE',  ( 5.599999999999998757, 6.472876824008161592E-16, -5.200000000000001066 ) ) ;
#7081 = DIRECTION ( 'NONE',  ( 0.000000000000000000, 0.000000000000000000, 1.000000000000000000 ) ) ;
#7082 =( REPRESENTATION_RELATIONSHIP ('NONE','NONE', #5328, #5848 ) REPRESENTATION_RELATIONSHIP_WITH_TRANSFORMATION ( #6849 )SHAPE_REPRESENTATION_RELATIONSHIP( ) );
#7083 = APPLICATION_PROTOCOL_DEFINITION ( 'draft international standard', 'automotive_design', 1998, #12976 ) ;
#7084 = CARTESIAN_POINT ( 'NONE',  ( 42.63976443033212860, 62.99948385550241170, 0.02388180880522514787 ) ) ;
#7085 = CARTESIAN_POINT ( 'NONE',  ( 56.66441430157296821, 60.09948385550240602, 2.141517661632100111 ) ) ;
#7086 = CIRCLE ( 'NONE', #7534, 2.500000000000000444 ) ;
#7087 = CARTESIAN_POINT ( 'NONE',  ( -4.000000000000000888, -1.539600717839011201, -3.300726591567081591 ) ) ;
#7088 = DIRECTION ( 'NONE',  ( 0.000000000000000000, 0.000000000000000000, 1.000000000000000000 ) ) ;
#7089 = CARTESIAN_POINT ( 'NONE',  ( 1.925929944387235853E-31, 15.00000000000001599, 9.000000000000000000 ) ) ;
#7090 = CARTESIAN_POINT ( 'NONE',  ( 52.25172492374527877, 49.40051614449766504, 7.007379884777203749 ) ) ;
#7091 = CARTESIAN_POINT ( 'NONE',  ( 51.97223112728254790, 54.39948385550241028, 5.992620115222778487 ) ) ;
#7092 = FACE_BOUND ( 'NONE', #11726, .T. ) ;
#7093 = ORIENTED_EDGE ( 'NONE', *, *, #9827, .T. ) ;
#7094 = ADVANCED_FACE ( 'NONE', ( #3240 ), #5520, .T. ) ;
#7095 = EDGE_LOOP ( 'NONE', ( #4354, #2303, #4150, #11317 ) ) ;
#7096 = ORIENTED_EDGE ( 'NONE', *, *, #7291, .T. ) ;
#7097 = CARTESIAN_POINT ( 'NONE',  ( -3.098410542199071749, -7.060458129626440815, -1.000000000000000000 ) ) ;
#7098 = DIRECTION ( 'NONE',  ( 0.000000000000000000, 0.000000000000000000, -1.000000000000000000 ) ) ;
#7099 = CARTESIAN_POINT ( 'NONE',  ( 6.541334219041339715, -5.921300567812618709, 0.03049376373817737351 ) ) ;
#7100 = CARTESIAN_POINT ( 'NONE',  ( 44.03140696652192787, 47.19948385550240744, -4.306917132069425058 ) ) ;
#7101 = FILL_AREA_STYLE_COLOUR ( '', #1162 ) ;
#7102 = EDGE_CURVE ( 'NONE', #4189, #3920, #1138, .T. ) ;
#7103 = CARTESIAN_POINT ( 'NONE',  ( 6.212060063025226064, 2.039954613758735658, -5.000000000000000000 ) ) ;
#7104 = CARTESIAN_POINT ( 'NONE',  ( 48.02776887271750184, 47.60051614449766078, 5.992620115222795363 ) ) ;
#7105 = DIRECTION ( 'NONE',  ( 0.000000000000000000, 0.4999999999999989453, -0.8660254037844391517 ) ) ;
#7106 = CARTESIAN_POINT ( 'NONE',  ( 55.94051828345050836, 57.79948385550238754, -4.345558710429104465 ) ) ;
#7107 = CARTESIAN_POINT ( 'NONE',  ( 54.09612160359786515, 53.69948385550240744, -5.676469297603166098 ) ) ;
#7108 = AXIS2_PLACEMENT_3D ( 'NONE', #12394, #7155, #4799 ) ;
#7109 = CIRCLE ( 'NONE', #6023, 1.500000000000001332 ) ;
#7110 = ORIENTED_EDGE ( 'NONE', *, *, #2427, .T. ) ;
#7111 = CARTESIAN_POINT ( 'NONE',  ( 49.97728705011488159, 51.49948385550240459, -7.000000000000000888 ) ) ;
#7112 = ORIENTED_EDGE ( 'NONE', *, *, #6628, .F. ) ;
#7113 = CARTESIAN_POINT ( 'NONE',  ( -13.67449106481168997, -13.83491329190049690, 9.000000000000000000 ) ) ;
#7114 = ORIENTED_EDGE ( 'NONE', *, *, #4870, .F. ) ;
#7115 = EDGE_CURVE ( 'NONE', #10183, #12550, #7539, .T. ) ;
#7116 = DIRECTION ( 'NONE',  ( -1.000000000000000000, 0.000000000000000000, 0.000000000000000000 ) ) ;
#7117 = AXIS2_PLACEMENT_3D ( 'NONE', #747, #3812, #10305 ) ;
#7118 = EDGE_CURVE ( 'NONE', #7909, #6904, #4898, .T. ) ;
#7119 = CARTESIAN_POINT ( 'NONE',  ( 0.4465819873852049926, -5.773502691896263528, -3.127607256515468906E-17 ) ) ;
#7120 = AXIS2_PLACEMENT_3D ( 'NONE', #13492, #559, #4042 ) ;
#7121 = CIRCLE ( 'NONE', #1351, 3.309499999999999886 ) ;
#7122 = DIRECTION ( 'NONE',  ( -0.000000000000000000, 0.000000000000000000, -1.000000000000000000 ) ) ;
#7123 = CARTESIAN_POINT ( 'NONE',  ( 53.54508667620424234, 58.70051614449765509, -4.840751629271188961 ) ) ;
#7124 = CARTESIAN_POINT ( 'NONE',  ( 4.211405965630455661, 2.460463115436283932, -3.751298928144577882 ) ) ;
#7125 = CARTESIAN_POINT ( 'NONE',  ( 54.68390685589033495, 61.69948385550240744, -6.485486291978119766 ) ) ;
#7126 = CARTESIAN_POINT ( 'NONE',  ( 44.03140696652192787, 61.19948385550239323, -4.306917132069425058 ) ) ;
#7127 = CARTESIAN_POINT ( 'NONE',  ( -0.1481481481481481122, -4.797713218419819903, -1.000000000000000000 ) ) ;
#7128 = CARTESIAN_POINT ( 'NONE',  ( 41.58830220609386430, 52.99948385550241170, 0.02388180880523263147 ) ) ;
#7129 = VECTOR ( 'NONE', #4683, 1000.000000000000000 ) ;
#7130 = EDGE_LOOP ( 'NONE', ( #12824, #11288 ) ) ;
#7131 = ORIENTED_EDGE ( 'NONE', *, *, #194, .F. ) ;
#7132 = AXIS2_PLACEMENT_3D ( 'NONE', #4586, #3478, #12801 ) ;
#7133 = ORIENTED_EDGE ( 'NONE', *, *, #1135, .F. ) ;
#7134 = CARTESIAN_POINT ( 'NONE',  ( -74.99999999999997158, 40.00000000000001421, 10.00000000000000000 ) ) ;
#7135 = ADVANCED_FACE ( 'NONE', ( #2188 ), #4208, .F. ) ;
#7136 = EDGE_CURVE ( 'NONE', #1508, #278, #7596, .T. ) ;
#7137 = CARTESIAN_POINT ( 'NONE',  ( 6.244297270354683960, 1.802013835206515036E-11, 5.105276777067893512 ) ) ;
#7138 = DIRECTION ( 'NONE',  ( -0.000000000000000000, -0.000000000000000000, 1.000000000000000000 ) ) ;
#7139 = DIRECTION ( 'NONE',  ( 0.000000000000000000, 0.000000000000000000, -1.000000000000000000 ) ) ;
#7140 = CARTESIAN_POINT ( 'NONE',  ( 44.30067958973596376, 62.89948385550240317, 1.875703265242204099 ) ) ;
#7141 = ADVANCED_FACE ( 'NONE', ( #11734 ), #9798, .F. ) ;
#7142 = CARTESIAN_POINT ( 'NONE',  ( 44.03140696652198471, 51.80051614449766362, 4.306917132069485454 ) ) ;
#7143 = CARTESIAN_POINT ( 'NONE',  ( 58.41169779390614281, 59.00051614449766646, 0.02388180880515032231 ) ) ;
#7144 = VECTOR ( 'NONE', #4009, 1000.000000000000000 ) ;
#7145 = CARTESIAN_POINT ( 'NONE',  ( -4.000000000000000000, 0.8730739991738342143, -3.223134629628428893 ) ) ;
#7146 = CARTESIAN_POINT ( 'NONE',  ( 45.27934281921082516, 49.70051614449766220, 6.458785618021089192 ) ) ;
#7148 = ORIENTED_EDGE ( 'NONE', *, *, #9478, .T. ) ;
#7147 = EDGE_LOOP ( 'NONE', ( #9149, #8825 ) ) ;
#7149 = CLOSED_SHELL ( 'NONE', ( #7407, #2056, #8232, #8754, #4723, #6640, #3726, #2805, #10242, #560, #2886, #4745, #6282, #9227, #11027, #10122, #7592, #3249, #11680, #9620, #12519, #12522, #12180, #10846, #12621, #3167, #9411, #9993, #1338, #2276, #6371, #9386 ) ) ;
#7150 = AXIS2_PLACEMENT_3D ( 'NONE', #12414, #8211, #714 ) ;
#7151 = ORIENTED_EDGE ( 'NONE', *, *, #13093, .F. ) ;
#7152 = ORIENTED_EDGE ( 'NONE', *, *, #7625, .F. ) ;
#7153 = CARTESIAN_POINT ( 'NONE',  ( 2.449293598294706513E-15, -20.00000000000000000, 9.000000000000000000 ) ) ;
#7154 = FACE_OUTER_BOUND ( 'NONE', #1826, .T. ) ;
#7155 = DIRECTION ( 'NONE',  ( 9.710251638871371392E-17, 5.969973981896233748E-17, 1.000000000000000000 ) ) ;
#7156 = PRODUCT_CONTEXT ( 'NONE', #3544, 'mechanical' ) ;
#7157 = CARTESIAN_POINT ( 'NONE',  ( 43.34962307344081012, 60.89948385550241028, 2.184720259617164650 ) ) ;
#7158 = CARTESIAN_POINT ( 'NONE',  ( 43.34962307344081012, 56.89948385550240317, 2.184720259617164650 ) ) ;
#7159 = CARTESIAN_POINT ( 'NONE',  ( -4.000000000000000000, -7.806255641895631925E-15, -3.142992957459232350 ) ) ;
#7160 = CARTESIAN_POINT ( 'NONE',  ( 7.500000000000003553, -20.00000000000000000, -20.00000000000000000 ) ) ;
#7161 = DIRECTION ( 'NONE',  ( -1.000000000000000000, -0.000000000000000000, -0.000000000000000000 ) ) ;
#7162 = EDGE_CURVE ( 'NONE', #12202, #4538, #10891, .T. ) ;
#7163 = CARTESIAN_POINT ( 'NONE',  ( 42.63976443033212860, 48.00051614449766646, -0.02388180880514948964 ) ) ;
#7164 = CARTESIAN_POINT ( 'NONE',  ( 46.45491332379572924, 55.29948385550240175, -4.840751629271157874 ) ) ;
#7165 = DIRECTION ( 'NONE',  ( -9.858538378746663627E-23, 5.031452844637890958E-23, -1.000000000000000000 ) ) ;
#7166 = AXIS2_PLACEMENT_3D ( 'NONE', #9442, #13642, #9974 ) ;
#7167 = VERTEX_POINT ( 'NONE', #7662 ) ;
#7168 = CARTESIAN_POINT ( 'NONE',  ( -29.99999999999999645, 0.000000000000000000, -10.00000000000000000 ) ) ;
#7169 = ORIENTED_EDGE ( 'NONE', *, *, #3769, .F. ) ;
#7170 = ORIENTED_EDGE ( 'NONE', *, *, #8802, .T. ) ;
#7171 = DIRECTION ( 'NONE',  ( -1.000000000000000000, 0.000000000000000000, 0.000000000000000000 ) ) ;
#7172 = CARTESIAN_POINT ( 'NONE',  ( 6.357976367241631621, 3.426708043487392885, -4.282301071214502208 ) ) ;
#7173 = EDGE_CURVE ( 'NONE', #12840, #12234, #11026, .T. ) ;
#7174 = DIRECTION ( 'NONE',  ( 0.000000000000000000, 0.000000000000000000, -1.000000000000000000 ) ) ;
#7175 = CARTESIAN_POINT ( 'NONE',  ( 2.000000000000000000, -0.8865213383406694847, 1.535500000000001419 ) ) ;
#7176 = CYLINDRICAL_SURFACE ( 'NONE', #7150, 4.799999999999999822 ) ;
#7177 = AXIS2_PLACEMENT_3D ( 'NONE', #7009, #11426, #13486 ) ;
#7178 = DIRECTION ( 'NONE',  ( -0.000000000000000000, -0.000000000000000000, -1.000000000000000000 ) ) ;
#7179 = CARTESIAN_POINT ( 'NONE',  ( 44.28664221472221385, 47.90051614449765793, 1.832500667257213722 ) ) ;
#7180 = FACE_OUTER_BOUND ( 'NONE', #5222, .T. ) ;
#7181 = VECTOR ( 'NONE', #8539, 1000.000000000000000 ) ;
#7182 = CARTESIAN_POINT ( 'NONE',  ( 45.90387839640214196, 56.69948385550240744, 5.676469297603166098 ) ) ;
#7183 = CARTESIAN_POINT ( 'NONE',  ( 57.36023556966787851, 53.99948385550239038, -0.02388180880522424582 ) ) ;
#7184 = EDGE_CURVE ( 'NONE', #5888, #6976, #8832, .T. ) ;
#7185 = VECTOR ( 'NONE', #8227, 1000.000000000000000 ) ;
#7186 = VERTEX_POINT ( 'NONE', #380 ) ;
#7187 = CARTESIAN_POINT ( 'NONE',  ( 47.70284917648453415, 47.39948385550238896, -6.992620115222774047 ) ) ;
#7188 = PRODUCT_RELATED_PRODUCT_CATEGORY ( 'part', '', ( #1011 ) ) ;
#7189 = VECTOR ( 'NONE', #3452, 1000.000000000000000 ) ;
#7190 = EDGE_LOOP ( 'NONE', ( #8311, #1699, #2995, #1666, #3825 ) ) ;
#7191 = DIRECTION ( 'NONE',  ( -1.734723475976807341E-16, -1.000000000000000000, 0.000000000000000000 ) ) ;
#7192 = EDGE_LOOP ( 'NONE', ( #2522, #5469, #13654, #5792 ) ) ;
#7193 = PLANE ( 'NONE',  #3642 ) ;
#7194 = CARTESIAN_POINT ( 'NONE',  ( 13.61000000000001009, 0.000000000000000000, 0.000000000000000000 ) ) ;
#7195 = CARTESIAN_POINT ( 'NONE',  ( 55.96859303347805081, 48.19948385550240744, 4.306917132069425058 ) ) ;
#7196 = CARTESIAN_POINT ( 'NONE',  ( 44.28664221472221385, 63.90051614449765793, 1.832500667257213722 ) ) ;
#7197 = CARTESIAN_POINT ( 'NONE',  ( -4.000000000000000000, 0.3987449864459974846, -0.01220643443059782861 ) ) ;
#7198 = VECTOR ( 'NONE', #11098, 1000.000000000000000 ) ;
#7199 = CARTESIAN_POINT ( 'NONE',  ( 57.61547081786812896, 60.09948385550240602, 2.450534656007040901 ) ) ;
#7200 = DIRECTION ( 'NONE',  ( 0.000000000000000000, 0.000000000000000000, 1.000000000000000000 ) ) ;
#7201 = CARTESIAN_POINT ( 'NONE',  ( 57.60143344285433642, 49.89948385550241028, -2.493737253992118319 ) ) ;
#7202 = VERTEX_POINT ( 'NONE', #13228 ) ;
#7203 = VERTEX_POINT ( 'NONE', #8904 ) ;
#7204 = VERTEX_POINT ( 'NONE', #1476 ) ;
#7205 = ADVANCED_FACE ( 'NONE', ( #9991 ), #12958, .T. ) ;
#7206 = LINE ( 'NONE', #12375, #5291 ) ;
#7207 = CARTESIAN_POINT ( 'NONE',  ( 4.030867648405251025, 2.329326259789668452, -2.965488570640744115 ) ) ;
#7208 = CARTESIAN_POINT ( 'NONE',  ( -2.000000000000006661, 3.464101615137750834, 0.000000000000000000 ) ) ;
#7209 = DIRECTION ( 'NONE',  ( -1.000000000000000000, -0.000000000000000000, -0.000000000000000000 ) ) ;
#7210 = CARTESIAN_POINT ( 'NONE',  ( 43.69122665457040000, 60.99948385550241170, 0.02388180880521036456 ) ) ;
#7211 = CARTESIAN_POINT ( 'NONE',  ( 50.02271294988505446, 56.50051614449766646, -7.000000000000000888 ) ) ;
#7212 = ADVANCED_FACE ( 'NONE', ( #2455 ), #510, .F. ) ;
#7213 = CARTESIAN_POINT ( 'NONE',  ( 45.31609314410960820, 60.30051614449767072, -6.485486291978072693 ) ) ;
#7214 = CARTESIAN_POINT ( 'NONE',  ( -3.999999999998910649, -1.658469974638591804, -3.531532913075256186 ) ) ;
#7215 = EDGE_CURVE ( 'NONE', #9204, #9576, #8964, .T. ) ;
#7216 = CARTESIAN_POINT ( 'NONE',  ( 47.42335538002180328, 50.40051614449766504, -8.007379884777206414 ) ) ;
#7217 = AXIS2_PLACEMENT_3D ( 'NONE', #9635, #291, #2295 ) ;
#7218 = EDGE_CURVE ( 'NONE', #10183, #10214, #3784, .T. ) ;
#7220 = ORIENTED_EDGE ( 'NONE', *, *, #3661, .F. ) ;
#7219 = ORIENTED_EDGE ( 'NONE', *, *, #3551, .T. ) ;
#7221 = ORIENTED_EDGE ( 'NONE', *, *, #6034, .F. ) ;
#7222 = ORIENTED_EDGE ( 'NONE', *, *, #3233, .T. ) ;
#7223 = DIRECTION ( 'NONE',  ( -1.000000000000000000, 0.000000000000000000, 0.000000000000000000 ) ) ;
#7224 = EDGE_CURVE ( 'NONE', #9006, #10405, #7799, .T. ) ;
#7225 = CARTESIAN_POINT ( 'NONE',  ( -11.49038105676659249, -12.50000000000003020, 9.000000000000000000 ) ) ;
#7226 = CARTESIAN_POINT ( 'NONE',  ( -3.574908632038010113E-15, 4.821944789745366222, -1.648146632869000427 ) ) ;
#7227 = CARTESIAN_POINT ( 'NONE',  ( 75.00000000000000000, 32.50000000000001421, 9.999999999999998224 ) ) ;
#7228 = SHAPE_DEFINITION_REPRESENTATION ( #11846, #8584 ) ;
#7229 = CARTESIAN_POINT ( 'NONE',  ( 45.86712807150323812, 63.29948385550240886, -5.649768623646098220 ) ) ;
#7230 = CARTESIAN_POINT ( 'NONE',  ( 50.02271294988512551, 60.49948385550240459, 7.000000000000000888 ) ) ;
#7231 = CARTESIAN_POINT ( 'NONE',  ( 44.03140696652198471, 57.80051614449766362, 4.306917132069485454 ) ) ;
#7232 = DIRECTION ( 'NONE',  ( 1.000000000000000000, 0.000000000000000000, 0.000000000000000000 ) ) ;
#7233 = DIRECTION ( 'NONE',  ( 0.000000000000000000, 0.000000000000000000, -1.000000000000000000 ) ) ;
#7234 = LINE ( 'NONE', #6205, #56 ) ;
#7235 = CARTESIAN_POINT ( 'NONE',  ( 44.03140696652198471, 53.80051614449766362, 4.306917132069485454 ) ) ;
#7236 = CARTESIAN_POINT ( 'NONE',  ( 44.30067958973596376, 50.89948385550240317, 1.875703265242204099 ) ) ;
#7237 = CARTESIAN_POINT ( 'NONE',  ( 1.925929944387235853E-31, 15.00000000000001599, 9.000000000000000000 ) ) ;
#7238 = ORIENTED_EDGE ( 'NONE', *, *, #3459, .F. ) ;
#7239 = DIRECTION ( 'NONE',  ( 0.000000000000000000, 0.8660254037844375974, -0.5000000000000018874 ) ) ;
#7240 = B_SPLINE_CURVE_WITH_KNOTS ( 'NONE', 3,
 ( #10457, #9362, #2997, #2928 ),
 .UNSPECIFIED., .F., .F.,
 ( 4, 4 ),
 ( 2.380739282168708963E-07, 0.002044882221487539717 ),
 .UNSPECIFIED. ) ;
#7241 = ORIENTED_EDGE ( 'NONE', *, *, #12236, .T. ) ;
#7242 = ORIENTED_EDGE ( 'NONE', *, *, #9892, .F. ) ;
#7243 = CYLINDRICAL_SURFACE ( 'NONE', #9470, 15.00000000000000000 ) ;
#7244 = LINE ( 'NONE', #6146, #6070 ) ;
#7245 = CARTESIAN_POINT ( 'NONE',  ( 6.420058897733096792, -2.891482565094587898, 5.008194711943423805 ) ) ;
#7246 = CARTESIAN_POINT ( 'NONE',  ( -9.999999999999998224, 15.00000000000001776, -9.999999999999998224 ) ) ;
#7247 = CARTESIAN_POINT ( 'NONE',  ( 56.30877334542961421, 47.00051614449766646, 0.02388180880515774693 ) ) ;
#7248 = CARTESIAN_POINT ( 'NONE',  ( 1.000000000000000000, -14.00000000000000000, 8.999999999999998224 ) ) ;
#7249 = CARTESIAN_POINT ( 'NONE',  ( 54.09612160359786515, 61.69948385550240744, -5.676469297603166098 ) ) ;
#7250 = CARTESIAN_POINT ( 'NONE',  ( 56.66441430157296821, 52.09948385550240602, 2.141517661632100111 ) ) ;
#7251 = EDGE_CURVE ( 'NONE', #11745, #6246, #2664, .T. ) ;
#7252 = ORIENTED_EDGE ( 'NONE', *, *, #1196, .F. ) ;
#7253 = CARTESIAN_POINT ( 'NONE',  ( 43.34962307344081012, 52.89948385550240317, 2.184720259617164650 ) ) ;
#7254 = AXIS2_PLACEMENT_3D ( 'NONE', #2773, #2627, #476 ) ;
#7255 = ORIENTED_EDGE ( 'NONE', *, *, #11336, .F. ) ;
#7256 = CARTESIAN_POINT ( 'NONE',  ( 20.00000000000000000, -20.00000000000000000, -23.00000000000000000 ) ) ;
#7257 = ORIENTED_EDGE ( 'NONE', *, *, #13527, .F. ) ;
#7258 = CARTESIAN_POINT ( 'NONE',  ( 0.000000000000000000, 0.000000000000000000, 0.000000000000000000 ) ) ;
#7259 = DIRECTION ( 'NONE',  ( -0.000000000000000000, -0.000000000000000000, -1.000000000000000000 ) ) ;
#7260 = CARTESIAN_POINT ( 'NONE',  ( -4.999999999999998224, -20.00000000000000000, 9.000000000000000000 ) ) ;
#7261 = CARTESIAN_POINT ( 'NONE',  ( 52.25172492374527877, 47.40051614449766504, 7.007379884777203749 ) ) ;
#7262 = VECTOR ( 'NONE', #12757, 1000.000000000000000 ) ;
#7263 = CARTESIAN_POINT ( 'NONE',  ( 6.270568613849412998, -3.932080789230354867, 3.401571648088637101 ) ) ;
#7264 = SHAPE_REPRESENTATION ( 'socket head cap screw_iso_ISO 4762 M4 x 10 - 10N', ( #430 ), #3078 ) ;
#7265 = CARTESIAN_POINT ( 'NONE',  ( 54.09612160359786515, 47.69948385550240744, -5.676469297603166098 ) ) ;
#7266 = DIRECTION ( 'NONE',  ( 0.000000000000000000, 0.000000000000000000, 1.000000000000000000 ) ) ;
#7267 = CARTESIAN_POINT ( 'NONE',  ( 1.567478505476134606E-15, 4.618802153517012066, -3.433295621305382905 ) ) ;
#7268 = CARTESIAN_POINT ( 'NONE',  ( 47.37792948025162332, 47.39948385550241028, -7.992620115222770494 ) ) ;
#7269 = ORIENTED_EDGE ( 'NONE', *, *, #40, .T. ) ;
#7270 = ORIENTED_EDGE ( 'NONE', *, *, #1265, .F. ) ;
#7271 = VERTEX_POINT ( 'NONE', #11866 ) ;
#7272 = AXIS2_PLACEMENT_3D ( 'NONE', #6960, #6145, #10338 ) ;
#7273 = EDGE_CURVE ( 'NONE', #1489, #5890, #10626, .T. ) ;
#7274 = CARTESIAN_POINT ( 'NONE',  ( 2.449293598294706513E-15, -20.00000000000000000, -50.00000000000000000 ) ) ;
#7275 = CIRCLE ( 'NONE', #11671, 2.649999999999985700 ) ;
#7276 = CYLINDRICAL_SURFACE ( 'NONE', #3148, 1.500000000000001332 ) ;
#7277 = CARTESIAN_POINT ( 'NONE',  ( 0.000000000000000000, -3.031088913245531202, 1.750000000000006439 ) ) ;
#7278 = CARTESIAN_POINT ( 'NONE',  ( 4.235886605889389145, 2.417314728048528760, -3.751161874094018245 ) ) ;
#7279 = CARTESIAN_POINT ( 'NONE',  ( 55.69932041026405045, 51.10051614449766078, 1.875703265242156359 ) ) ;
#7280 = CARTESIAN_POINT ( 'NONE',  ( 56.65037692655921120, 57.10051614449766078, 2.184720259617097593 ) ) ;
#7281 = EDGE_CURVE ( 'NONE', #4712, #2490, #10056, .T. ) ;
#7282 = CARTESIAN_POINT ( 'NONE',  ( 43.18075615816994173, 59.80051614449766362, 4.924951120819380357 ) ) ;
#7283 = CIRCLE ( 'NONE', #1288, 7.500000000000000888 ) ;
#7284 = DIRECTION ( 'NONE',  ( -0.000000000000000000, -0.000000000000000000, -1.000000000000000000 ) ) ;
#7285 = CARTESIAN_POINT ( 'NONE',  ( 52.57664461997821093, 51.40051614449767214, 8.007379884777206414 ) ) ;
#7286 = AXIS2_PLACEMENT_3D ( 'NONE', #12938, #7640, #2364 ) ;
#7288 = VERTEX_POINT ( 'NONE', #1340 ) ;
#7287 = ORIENTED_EDGE ( 'NONE', *, *, #4439, .T. ) ;
#7289 = VERTEX_POINT ( 'NONE', #2387 ) ;
#7290 = VERTEX_POINT ( 'NONE', #2593 ) ;
#7291 = EDGE_CURVE ( 'NONE', #9858, #6669, #9725, .T. ) ;
#7292 = EDGE_CURVE ( 'NONE', #3770, #10906, #4784, .T. ) ;
#7293 = ORIENTED_EDGE ( 'NONE', *, *, #4410, .T. ) ;
#7295 = VECTOR ( 'NONE', #5431, 1000.000000000000000 ) ;
#7294 = CARTESIAN_POINT ( 'NONE',  ( -74.99999999999998579, -2.602085213965210642E-14, 0.000000000000000000 ) ) ;
#7296 = EDGE_CURVE ( 'NONE', #11340, #3318, #9924, .T. ) ;
#7297 = CARTESIAN_POINT ( 'NONE',  ( 4.175813232069146785, -2.061359961916366057, 3.570380186727398542 ) ) ;
#7298 = CARTESIAN_POINT ( 'NONE',  ( -62.49999999999997158, 32.50000000000001421, -9.999999999999998224 ) ) ;
#7299 = ADVANCED_FACE ( 'NONE', ( #9862 ), #4681, .F. ) ;
#7300 = CARTESIAN_POINT ( 'NONE',  ( 56.65037692655918988, 63.89948385550239607, -2.184720259617163762 ) ) ;
#7301 = AXIS2_PLACEMENT_3D ( 'NONE', #2713, #9904, #6937 ) ;
#7302 = DIRECTION ( 'NONE',  ( -0.000000000000000000, -0.000000000000000000, 1.000000000000000000 ) ) ;
#7303 = CARTESIAN_POINT ( 'NONE',  ( 49.97728705011495265, 59.50051614449765935, 7.000000000000000888 ) ) ;
#7304 = DIRECTION ( 'NONE',  ( -1.000000000000000000, 0.000000000000000000, 0.000000000000000000 ) ) ;
#7305 = DIRECTION ( 'NONE',  ( 1.224646799147353207E-16, 1.000000000000000000, 0.000000000000000000 ) ) ;
#7306 = CARTESIAN_POINT ( 'NONE',  ( 4.086262629614029862, 4.082406995609985323, 0.07093633357110586124 ) ) ;
#7307 = CARTESIAN_POINT ( 'NONE',  ( 43.34962307344078880, 48.10051614449766078, -2.184720259617096705 ) ) ;
#7308 = CARTESIAN_POINT ( 'NONE',  ( 55.08986747509847248, 61.79948385550240175, -3.727524721679197572 ) ) ;
#7309 = AXIS2_PLACEMENT_3D ( 'NONE', #10965, #3512, #6701 ) ;
#7310 = CARTESIAN_POINT ( 'NONE',  ( -4.000000000000000000, 2.309401076758498483, -0.4999999999999927280 ) ) ;
#7311 = ORIENTED_EDGE ( 'NONE', *, *, #2913, .T. ) ;
#7312 = PLANE ( 'NONE',  #783 ) ;
#7313 = ORIENTED_EDGE ( 'NONE', *, *, #10013, .F. ) ;
#7314 = ORIENTED_EDGE ( 'NONE', *, *, #3817, .F. ) ;
#7315 = DIRECTION ( 'NONE',  ( 0.000000000000000000, 1.000000000000000000, 0.000000000000000000 ) ) ;
#7316 = CARTESIAN_POINT ( 'NONE',  ( 6.095473853218515536, 4.853892138986921623, -1.592812200815479695 ) ) ;
#7317 = CARTESIAN_POINT ( 'NONE',  ( 6.541171370350062020, -2.986177670315871335, 5.112746295475706582 ) ) ;
#7318 =( GEOMETRIC_REPRESENTATION_CONTEXT ( 3 ) GLOBAL_UNCERTAINTY_ASSIGNED_CONTEXT ( ( #1944 ) ) GLOBAL_UNIT_ASSIGNED_CONTEXT ( ( #6590, #1375, #13065 ) ) REPRESENTATION_CONTEXT ( 'NONE', 'WORKASPACE' ) );
#7319 = FILL_AREA_STYLE ('',( #8351 ) ) ;
#7320 = CARTESIAN_POINT ( 'NONE',  ( 44.05948171654949874, 46.79948385550238754, 4.345558710429105354 ) ) ;
#7321 = VECTOR ( 'NONE', #10976, 1000.000000000000000 ) ;
#7322 = DIRECTION ( 'NONE',  ( -1.000000000000000000, 0.000000000000000000, 0.000000000000000000 ) ) ;
#7323 = CARTESIAN_POINT ( 'NONE',  ( 49.97728705011494554, 49.50051614449766646, 6.000000000000000888 ) ) ;
#7324 = DIRECTION ( 'NONE',  ( 1.000000000000000000, 0.000000000000000000, 0.000000000000000000 ) ) ;
#7325 = CARTESIAN_POINT ( 'NONE',  ( 57.36023556966787851, 61.99948385550241170, -0.02388180880522424582 ) ) ;
#7326 = CARTESIAN_POINT ( 'NONE',  ( 44.03140696652192787, 55.19948385550238612, -4.306917132069425058 ) ) ;
#7327 = VERTEX_POINT ( 'NONE', #2526 ) ;
#7328 = VERTEX_POINT ( 'NONE', #6758 ) ;
#7329 = CARTESIAN_POINT ( 'NONE',  ( 3.880214671983734043, -0.7309020039772819999, 3.500000000000000444 ) ) ;
#7330 = DIRECTION ( 'NONE',  ( -1.000000000000000000, 0.000000000000000000, 0.000000000000000000 ) ) ;
#7331 = CARTESIAN_POINT ( 'NONE',  ( 4.630153689607048761, 6.577590292450083844E-16, 5.371010071662833063 ) ) ;
#7332 = EDGE_CURVE ( 'NONE', #10855, #9257, #2289, .T. ) ;
#7333 = DIRECTION ( 'NONE',  ( -1.000000000000000000, 0.000000000000000000, 0.000000000000000000 ) ) ;
#7334 = CARTESIAN_POINT ( 'NONE',  ( 56.66441430157296821, 46.09948385550240602, 2.141517661632100111 ) ) ;
#7335 = AXIS2_PLACEMENT_3D ( 'NONE', #3644, #445, #11099 ) ;
#7336 = CARTESIAN_POINT ( 'NONE',  ( 55.94051828345053679, 47.20051614449766220, 4.345558710429044069 ) ) ;
#7337 = CARTESIAN_POINT ( 'NONE',  ( 2.449293598294706513E-15, -20.00000000000000000, 9.000000000000000000 ) ) ;
#7338 = CARTESIAN_POINT ( 'NONE',  ( 47.74827507625478518, 46.59948385550239891, 7.007379884777227730 ) ) ;
#7339 = DIRECTION ( 'NONE',  ( 1.000000000000000000, 0.000000000000000000, 0.000000000000000000 ) ) ;
#7340 = CARTESIAN_POINT ( 'NONE',  ( 43.20883090819745576, 56.79948385550240175, 4.963592699179006473 ) ) ;
#7341 = ORIENTED_EDGE ( 'NONE', *, *, #8111, .T. ) ;
#7342 = CIRCLE ( 'NONE', #10850, 1.500000000000001332 ) ;
#7343 = ADVANCED_BREP_SHAPE_REPRESENTATION ( '', ( #1029, #430 ), #9694 ) ;
#7344 = VERTEX_POINT ( 'NONE', #11168 ) ;
#7345 = CIRCLE ( 'NONE', #7547, 2.499999999999999556 ) ;
#7346 = AXIS2_PLACEMENT_3D ( 'NONE', #8906, #3707, #13100 ) ;
#7347 = FACE_OUTER_BOUND ( 'NONE', #3517, .T. ) ;
#7348 = DIRECTION ( 'NONE',  ( -0.000000000000000000, -0.000000000000000000, 1.000000000000000000 ) ) ;
#7349 = CARTESIAN_POINT ( 'NONE',  ( 6.506891779418575439, -5.826362946429633816, -0.09155664655282159947 ) ) ;
#7350 = DIRECTION ( 'NONE',  ( 1.000000000000000000, 0.000000000000000000, 0.000000000000000000 ) ) ;
#7351 = CARTESIAN_POINT ( 'NONE',  ( 44.28664221472221385, 49.90051614449766504, 1.832500667257213722 ) ) ;
#7352 = CARTESIAN_POINT ( 'NONE',  ( 47.70284917648459810, 59.60051614449765367, 6.992620115222797139 ) ) ;
#7353 = CARTESIAN_POINT ( 'NONE',  ( 58.41169779390614281, 47.99948385550239038, -0.02388180880523160798 ) ) ;
#7354 = VECTOR ( 'NONE', #7348, 1000.000000000000000 ) ;
#7355 = CARTESIAN_POINT ( 'NONE',  ( -4.000000000000000000, 2.511478553582031203, -3.469254451724764543 ) ) ;
#7356 = CARTESIAN_POINT ( 'NONE',  ( 57.60143344285435774, 59.10051614449766078, 2.493737253992045044 ) ) ;
#7357 = ADVANCED_FACE ( 'NONE', ( #852 ), #9715, .F. ) ;
#7358 = EDGE_LOOP ( 'NONE', ( #6655, #2994, #4014, #11250, #9358 ) ) ;
#7359 = ORIENTED_EDGE ( 'NONE', *, *, #2118, .F. ) ;
#7360 = EDGE_LOOP ( 'NONE', ( #7152, #131, #1334, #9422 ) ) ;
#7361 = ADVANCED_FACE ( 'NONE', ( #1903 ), #11384, .F. ) ;
#7362 = PLANE ( 'NONE',  #6912 ) ;
#7363 = FILL_AREA_STYLE_COLOUR ( '', #11875 ) ;
#7364 = CARTESIAN_POINT ( 'NONE',  ( -29.99999999999999645, -40.00000000000000000, 10.00000000000000000 ) ) ;
#7365 = CARTESIAN_POINT ( 'NONE',  ( 3.806834918298644066, 1.084202172485504434E-15, 3.500000000000000000 ) ) ;
#7366 = VECTOR ( 'NONE', #1382, 1000.000000000000000 ) ;
#7367 = CARTESIAN_POINT ( 'NONE',  ( 53.54508667620428497, 50.29948385550240886, 4.840751629271157874 ) ) ;
#7368 = CARTESIAN_POINT ( 'NONE',  ( 1.925929944387235853E-31, 15.00000000000001599, -15.00000000000000000 ) ) ;
#7369 = CARTESIAN_POINT ( 'NONE',  ( 52.62207051974829852, 48.60051614449766788, -7.992620115222797139 ) ) ;
#7370 = CARTESIAN_POINT ( 'NONE',  ( 6.244297270353399654, -0.9889575675955545320, 5.105276777067856209 ) ) ;
#7371 = CYLINDRICAL_SURFACE ( 'NONE', #10732, 2.649999999999988365 ) ;
#7372 = CARTESIAN_POINT ( 'NONE',  ( 3.974175853610027342, 3.450041667725633143, -1.156004144283977908 ) ) ;
#7373 = CARTESIAN_POINT ( 'NONE',  ( 57.36023556966787851, 49.00051614449763804, 0.02388180880515038476 ) ) ;
#7374 = CARTESIAN_POINT ( 'NONE',  ( 44.88205777487398507, 57.19948385550241454, -3.688883143319540814 ) ) ;
#7375 = PLANE ( 'NONE',  #2746 ) ;
#7376 = VERTEX_POINT ( 'NONE', #11449 ) ;
#7377 = PLANE ( 'NONE',  #10365 ) ;
#7378 = VERTEX_POINT ( 'NONE', #3912 ) ;
#7379 = CARTESIAN_POINT ( 'NONE',  ( -74.99999999999997158, 7.499999999999971578, -10.00000000000000000 ) ) ;
#7380 = CARTESIAN_POINT ( 'NONE',  ( 1.925929944387235853E-31, 15.00000000000001599, -9.000000000000001776 ) ) ;
#7381 = EDGE_CURVE ( 'NONE', #7922, #11193, #12617, .T. ) ;
#7382 = CARTESIAN_POINT ( 'NONE',  ( 4.170895651974849017, 2.054890354522707074, -3.559174498016318910 ) ) ;
#7383 = CARTESIAN_POINT ( 'NONE',  ( 55.96859303347804371, 52.19948385550240033, 4.306917132069425946 ) ) ;
#7384 = CYLINDRICAL_SURFACE ( 'NONE', #1088, 5.000000000000000888 ) ;
#7385 = CARTESIAN_POINT ( 'NONE',  ( 46.49166364869456913, 54.30051614449765651, -4.867452303228181343 ) ) ;
#7386 = DIRECTION ( 'NONE',  ( -0.5000000000000019984, -0.8660254037844375974, 0.000000000000000000 ) ) ;
#7387 = CARTESIAN_POINT ( 'NONE',  ( 56.66441430157296821, 62.09948385550239891, 2.141517661632100111 ) ) ;
#7388 = CARTESIAN_POINT ( 'NONE',  ( 56.66441430157296821, 64.09948385550239891, 2.141517661632100111 ) ) ;
#7389 = CARTESIAN_POINT ( 'NONE',  ( 57.36023556966787851, 57.99948385550239038, -0.02388180880522424582 ) ) ;
#7390 = ORIENTED_EDGE ( 'NONE', *, *, #4582, .F. ) ;
#7391 = EDGE_CURVE ( 'NONE', #3730, #8238, #3843, .T. ) ;
#7392 = EDGE_CURVE ( 'NONE', #12054, #9060, #1974, .T. ) ;
#7393 = ORIENTED_EDGE ( 'NONE', *, *, #6959, .T. ) ;
#7394 = CARTESIAN_POINT ( 'NONE',  ( 20.00000000000000000, -14.99999999999999289, -23.00000000000000000 ) ) ;
#7395 = AXIS2_PLACEMENT_3D ( 'NONE', #5288, #1174, #6528 ) ;
#7396 = CARTESIAN_POINT ( 'NONE',  ( 1.411581201560190495E-15, 4.862606272033091592, -3.745885042887436622 ) ) ;
#7397 = CARTESIAN_POINT ( 'NONE',  ( 3.961551342853522950, -3.742715940867789026, 0.5174258321190450260 ) ) ;
#7398 = DIRECTION ( 'NONE',  ( 0.000000000000000000, 0.000000000000000000, 1.000000000000000000 ) ) ;
#7399 = CARTESIAN_POINT ( 'NONE',  ( 57.36023556966787851, 45.99948385550239749, -0.02388180880522424582 ) ) ;
#7400 = AXIS2_PLACEMENT_3D ( 'NONE', #13156, #3636, #565 ) ;
#7401 = CARTESIAN_POINT ( 'NONE',  ( 44.03140696652198471, 47.80051614449764230, 4.306917132069485454 ) ) ;
#7402 = CARTESIAN_POINT ( 'NONE',  ( 12.99038105676649835, -12.49999999999984901, -9.000000000000000000 ) ) ;
#7403 = CIRCLE ( 'NONE', #965, 15.00000000000000000 ) ;
#7404 = CARTESIAN_POINT ( 'NONE',  ( 49.97728705011486738, 65.49948385550240459, -8.000000000000001776 ) ) ;
#7405 = CARTESIAN_POINT ( 'NONE',  ( 3.129923130707922496, -23.63917314727666152, -9.999999999999994671 ) ) ;
#7406 = AXIS2_PLACEMENT_3D ( 'NONE', #11543, #943, #13523 ) ;
#7407 = ADVANCED_FACE ( 'NONE', ( #6078 ), #12278, .F. ) ;
#7408 = CARTESIAN_POINT ( 'NONE',  ( 57.60143344285433642, 57.89948385550241028, -2.493737253992118319 ) ) ;
#7409 = ORIENTED_EDGE ( 'NONE', *, *, #5699, .F. ) ;
#7410 = VECTOR ( 'NONE', #5180, 1000.000000000000114 ) ;
#7411 = B_SPLINE_CURVE_WITH_KNOTS ( 'NONE', 3,
 ( #3411, #11838, #8535, #7698, #5365 ),
 .UNSPECIFIED., .F., .F.,
 ( 4, 1, 4 ),
 ( 0.000000000000000000, 0.002886751345948131153, 0.005773502691896262307 ),
 .UNSPECIFIED. ) ;
#7412 = ORIENTED_EDGE ( 'NONE', *, *, #2346, .T. ) ;
#7413 = DIRECTION ( 'NONE',  ( 1.000000000000000000, 3.469446951953615175E-16, 0.000000000000000000 ) ) ;
#7414 = FACE_OUTER_BOUND ( 'NONE', #3113, .T. ) ;
#7415 = FACE_OUTER_BOUND ( 'NONE', #12372, .T. ) ;
#7416 = CIRCLE ( 'NONE', #12697, 9.999999999999998224 ) ;
#7417 = DIRECTION ( 'NONE',  ( 1.000000000000000000, 3.469446951953615175E-16, 0.000000000000000000 ) ) ;
#7418 = CARTESIAN_POINT ( 'NONE',  ( 44.88205777487401349, 49.80051614449765651, 3.688883143319584779 ) ) ;
#7419 = CARTESIAN_POINT ( 'NONE',  ( 57.36023556966787851, 59.00051614449765935, 0.02388180880515038476 ) ) ;
#7420 = CARTESIAN_POINT ( 'NONE',  ( 49.97728705011486738, 49.49948385550241170, -8.000000000000001776 ) ) ;
#7421 = CARTESIAN_POINT ( 'NONE',  ( 4.175075985190098926, -4.120741555260250877, 2.761631486132788719E-14 ) ) ;
#7422 = CARTESIAN_POINT ( 'NONE',  ( 49.97728705011495265, 59.50051614449765935, 8.000000000000001776 ) ) ;
#7423 = ORIENTED_EDGE ( 'NONE', *, *, #8708, .F. ) ;
#7424 = ORIENTED_EDGE ( 'NONE', *, *, #8680, .F. ) ;
#7425 = ORIENTED_EDGE ( 'NONE', *, *, #11433, .T. ) ;
#7426 = LINE ( 'NONE', #10593, #5815 ) ;
#7427 = CARTESIAN_POINT ( 'NONE',  ( 6.495567275915088423, 2.917443832164887230, -5.053160945538039961 ) ) ;
#7428 = CARTESIAN_POINT ( 'NONE',  ( -74.99999999999997158, 40.00000000000001421, -10.00000000000000000 ) ) ;
#7429 = FACE_OUTER_BOUND ( 'NONE', #9065, .T. ) ;
#7430 = DIRECTION ( 'NONE',  ( 0.000000000000000000, 1.000000000000000000, 0.000000000000000000 ) ) ;
#7431 = CARTESIAN_POINT ( 'NONE',  ( 56.30877334542961421, 47.99948385550239038, -0.02388180880520959434 ) ) ;
#7432 = CARTESIAN_POINT ( 'NONE',  ( 4.175813232069147674, 2.061359961916367833, 3.570380186727398097 ) ) ;
#7433 = CARTESIAN_POINT ( 'NONE',  ( 44.05948171654945611, 64.20051614449765509, -4.345558710429044069 ) ) ;
#7434 = AXIS2_PLACEMENT_3D ( 'NONE', #10400, #8267, #8197 ) ;
#7435 = CARTESIAN_POINT ( 'NONE',  ( 4.000000000000000000, 2.309401076758497151, -3.433295621305379353 ) ) ;
#7436 = CARTESIAN_POINT ( 'NONE',  ( -6.259644161404860030E-16, -4.618802153517027165, -5.000000000000000000 ) ) ;
#7437 = CARTESIAN_POINT ( 'NONE',  ( 55.96859303347802239, 58.80051614449764941, -4.306917132069484566 ) ) ;
#7438 = CARTESIAN_POINT ( 'NONE',  ( 51.92680522751233951, 57.59948385550240602, -6.007379884777223289 ) ) ;
#7439 = CARTESIAN_POINT ( 'NONE',  ( 0.000000000000000000, 20.00000000000001421, 9.999999999999998224 ) ) ;
#7440 = VERTEX_POINT ( 'NONE', #5103 ) ;
#7441 = DIRECTION ( 'NONE',  ( 1.000000000000000000, 0.000000000000000000, 0.000000000000000000 ) ) ;
#7442 = ORIENTED_EDGE ( 'NONE', *, *, #1464, .F. ) ;
#7443 = DIRECTION ( 'NONE',  ( 0.000000000000000000, 0.000000000000000000, 1.000000000000000000 ) ) ;
#7444 = CYLINDRICAL_SURFACE ( 'NONE', #5404, 1.500000000000001332 ) ;
#7445 = CARTESIAN_POINT ( 'NONE',  ( 4.114405500665261783, 2.025575754679710627, -3.508400121684937645 ) ) ;
#7446 = AXIS2_PLACEMENT_3D ( 'NONE', #7476, #8444, #6181 ) ;
#7447 = CARTESIAN_POINT ( 'NONE',  ( 50.02271294988512551, 52.49948385550240459, 7.000000000000000888 ) ) ;
#7448 = CARTESIAN_POINT ( 'NONE',  ( -0.2500000000000000000, -8.096141056083446585, -1.000000000000000000 ) ) ;
#7449 = CARTESIAN_POINT ( 'NONE',  ( 53.50833635130544508, 49.30051614449766362, 4.867452303228181343 ) ) ;
#7450 = EDGE_CURVE ( 'NONE', #8931, #12388, #453, .T. ) ;
#7451 = FACE_OUTER_BOUND ( 'NONE', #13322, .T. ) ;
#7452 = CARTESIAN_POINT ( 'NONE',  ( 42.63976443033212860, 62.99948385550241170, 0.02388180880522514787 ) ) ;
#7453 = CARTESIAN_POINT ( 'NONE',  ( 6.452281807715811723, -5.797857616945994330, 1.289641217033754180E-15 ) ) ;
#7454 = CARTESIAN_POINT ( 'NONE',  ( 45.86712807150323812, 59.29948385550240175, -5.649768623646098220 ) ) ;
#7455 = ORIENTED_EDGE ( 'NONE', *, *, #11357, .F. ) ;
#7456 = ORIENTED_EDGE ( 'NONE', *, *, #6449, .T. ) ;
#7457 = PLANE ( 'NONE',  #10773 ) ;
#7458 = ADVANCED_FACE ( 'NONE', ( #13436 ), #3018, .T. ) ;
#7459 = CARTESIAN_POINT ( 'NONE',  ( 0.000000000000000000, 0.000000000000000000, 0.000000000000000000 ) ) ;
#7460 = CARTESIAN_POINT ( 'NONE',  ( -2.000000000000006661, 3.464101615137750834, 0.000000000000000000 ) ) ;
#7461 = EDGE_CURVE ( 'NONE', #12172, #651, #10545, .T. ) ;
#7462 = PLANE ( 'NONE',  #9813 ) ;
#7463 = ADVANCED_FACE ( 'NONE', ( #1124 ), #12554, .F. ) ;
#7464 = DIRECTION ( 'NONE',  ( -0.000000000000000000, 0.000000000000000000, 1.000000000000000000 ) ) ;
#7465 = CARTESIAN_POINT ( 'NONE',  ( 52.29715082351538769, 48.60051614449766788, -6.992620115222796251 ) ) ;
#7466 = EDGE_CURVE ( 'NONE', #3434, #4810, #6933, .T. ) ;
#7467 = DIRECTION ( 'NONE',  ( -0.000000000000000000, -0.000000000000000000, 1.000000000000000000 ) ) ;
#7468 = CARTESIAN_POINT ( 'NONE',  ( 52.62207051974839089, 64.39948385550239607, 7.992620115222770494 ) ) ;
#7469 = CARTESIAN_POINT ( 'NONE',  ( -7.500000000000013323, -7.009618943233427935, -9.000000000000000000 ) ) ;
#7470 = CARTESIAN_POINT ( 'NONE',  ( 49.97728705011486738, 57.49948385550241170, -8.000000000000001776 ) ) ;
#7471 = EDGE_LOOP ( 'NONE', ( #8323, #523, #6108 ) ) ;
#7472 = ORIENTED_EDGE ( 'NONE', *, *, #3908, .T. ) ;
#7473 = CARTESIAN_POINT ( 'NONE',  ( 0.3126073911696407026, -2.020725942163686728, 3.500000000000000444 ) ) ;
#7474 = AXIS2_PLACEMENT_3D ( 'NONE', #11199, #672, #1510 ) ;
#7475 = LINE ( 'NONE', #10648, #12804 ) ;
#7476 = CARTESIAN_POINT ( 'NONE',  ( 2.000000000000000000, 0.000000000000000000, 0.000000000000000000 ) ) ;
#7477 = CARTESIAN_POINT ( 'NONE',  ( 53.50833635130544508, 45.30051614449766362, 4.867452303228181343 ) ) ;
#7478 = ADVANCED_FACE ( 'NONE', ( #9512 ), #9579, .F. ) ;
#7479 = CARTESIAN_POINT ( 'NONE',  ( 44.05948171654945611, 58.20051614449764799, -4.345558710429044069 ) ) ;
#7480 = CARTESIAN_POINT ( 'NONE',  ( 56.79116909180255135, 47.79948385550240886, -4.963592699179005585 ) ) ;
#7481 = CARTESIAN_POINT ( 'NONE',  ( 0.9183817310753817909, -24.91493387504115020, 9.000000000000000000 ) ) ;
#7482 = CARTESIAN_POINT ( 'NONE',  ( 47.37792948025170858, 59.60051614449765367, 7.992620115222797139 ) ) ;
#7483 = ORIENTED_EDGE ( 'NONE', *, *, #2362, .T. ) ;
#7484 = AXIS2_PLACEMENT_3D ( 'NONE', #927, #13437, #1975 ) ;
#7485 = ORIENTED_EDGE ( 'NONE', *, *, #777, .T. ) ;
#7486 = ORIENTED_EDGE ( 'NONE', *, *, #260, .T. ) ;
#7487 = LINE ( 'NONE', #11692, #5597 ) ;
#7488 = CARTESIAN_POINT ( 'NONE',  ( -9.999999999999994671, 20.00000000000001421, 15.00000000000000000 ) ) ;
#7489 = PLANE ( 'NONE',  #13557 ) ;
#7490 = PLANE ( 'NONE',  #2682 ) ;
#7491 = ADVANCED_FACE ( 'NONE', ( #2169 ), #2042, .T. ) ;
#7492 = CARTESIAN_POINT ( 'NONE',  ( 51.92680522751233951, 47.59948385550239891, -6.007379884777223289 ) ) ;
#7493 = EDGE_CURVE ( 'NONE', #6669, #13462, #1449, .T. ) ;
#7494 = CARTESIAN_POINT ( 'NONE',  ( 43.34962307344081012, 62.89948385550241028, 2.184720259617164650 ) ) ;
#7495 = CARTESIAN_POINT ( 'NONE',  ( 57.60143344285435774, 47.10051614449766078, 2.493737253992045044 ) ) ;
#7496 = CIRCLE ( 'NONE', #2182, 2.200000000000001066 ) ;
#7497 = CARTESIAN_POINT ( 'NONE',  ( -20.00000000000000000, -19.99999999999999289, -12.00000000000000000 ) ) ;
#7498 = CARTESIAN_POINT ( 'NONE',  ( -11.49038105676654453, -27.50000000000006040, 9.000000000000000000 ) ) ;
#7499 = CARTESIAN_POINT ( 'NONE',  ( 57.36023556966787851, 59.00051614449765935, 0.02388180880515038476 ) ) ;
#7500 = CARTESIAN_POINT ( 'NONE',  ( 53.54508667620428497, 60.29948385550240175, 4.840751629271157874 ) ) ;
#7501 = DIRECTION ( 'NONE',  ( 0.000000000000000000, -0.5000000000000001110, 0.8660254037844387076 ) ) ;
#7502 = ORIENTED_EDGE ( 'NONE', *, *, #7296, .T. ) ;
#7503 = DIRECTION ( 'NONE',  ( 0.000000000000000000, 0.000000000000000000, -1.000000000000000000 ) ) ;
#7504 = EDGE_LOOP ( 'NONE', ( #10712, #3365, #11928, #6122, #7096, #2856, #760 ) ) ;
#7505 = CARTESIAN_POINT ( 'NONE',  ( 62.49999999999998579, 40.00000000000001421, 9.999999999999998224 ) ) ;
#7506 = DIRECTION ( 'NONE',  ( -1.000000000000000000, 0.000000000000000000, -0.000000000000000000 ) ) ;
#7507 = LINE ( 'NONE', #11715, #8644 ) ;
#7508 = SURFACE_SIDE_STYLE ('',( #4457 ) ) ;
#7509 = CARTESIAN_POINT ( 'NONE',  ( 57.36023556966787851, 47.99948385550239038, -0.02388180880522424582 ) ) ;
#7510 = AXIS2_PLACEMENT_3D ( 'NONE', #428, #7782, #8886 ) ;
#7511 = VECTOR ( 'NONE', #4621, 1000.000000000000000 ) ;
#7512 = CARTESIAN_POINT ( 'NONE',  ( 0.000000000000000000, 0.000000000000000000, -4.484454397937119197 ) ) ;
#7513 = CARTESIAN_POINT ( 'NONE',  ( 55.69932041026405045, 49.10051614449766788, 1.875703265242156359 ) ) ;
#7514 = CARTESIAN_POINT ( 'NONE',  ( 2.385244779468109755E-15, -20.00000000000000000, -9.999999999999994671 ) ) ;
#7515 = LINE ( 'NONE', #2111, #8159 ) ;
#7516 = DIRECTION ( 'NONE',  ( 0.000000000000000000, 0.000000000000000000, -1.000000000000000000 ) ) ;
#7517 = CARTESIAN_POINT ( 'NONE',  ( 45.90387839640214196, 56.69948385550240744, 5.676469297603166098 ) ) ;
#7518 = CARTESIAN_POINT ( 'NONE',  ( 4.799999999999999822, 0.000000000000000000, -1.000000000000000000 ) ) ;
#7519 = EDGE_CURVE ( 'NONE', #13554, #12511, #11593, .T. ) ;
#7520 = ORIENTED_EDGE ( 'NONE', *, *, #7910, .F. ) ;
#7521 = EDGE_LOOP ( 'NONE', ( #3112, #2247 ) ) ;
#7522 = EDGE_LOOP ( 'NONE', ( #5862, #2299 ) ) ;
#7523 = CARTESIAN_POINT ( 'NONE',  ( -4.140404888673278272, -2.228338276487456415, -3.686887068327035166 ) ) ;
#7524 = CIRCLE ( 'NONE', #9067, 1.500000000000000666 ) ;
#7525 = EDGE_CURVE ( 'NONE', #9611, #690, #4325, .T. ) ;
#7526 = DIRECTION ( 'NONE',  ( -3.469446951953611033E-15, 1.000000000000000000, 0.000000000000000000 ) ) ;
#7527 = CARTESIAN_POINT ( 'NONE',  ( 1.000000000000000444, -15.10102051443364246, 15.00000000000000355 ) ) ;
#7528 = CARTESIAN_POINT ( 'NONE',  ( -62.49999999999997158, 45.00000000000001421, -9.999999999999998224 ) ) ;
#7529 = CARTESIAN_POINT ( 'NONE',  ( 56.65037692655918988, 51.89948385550241028, -2.184720259617163762 ) ) ;
#7530 = CARTESIAN_POINT ( 'NONE',  ( 54.13287192849671214, 46.70051614449766220, -5.649768623646139964 ) ) ;
#7531 = FACE_OUTER_BOUND ( 'NONE', #8916, .T. ) ;
#7532 = CARTESIAN_POINT ( 'NONE',  ( 43.20883090819745576, 64.79948385550240175, 4.963592699179006473 ) ) ;
#7533 = CARTESIAN_POINT ( 'NONE',  ( 50.00000000000000000, 15.00000000000000000, 0.000000000000000000 ) ) ;
#7534 = AXIS2_PLACEMENT_3D ( 'NONE', #5742, #11883, #8850 ) ;
#7535 = CARTESIAN_POINT ( 'NONE',  ( 43.18075615816989199, 55.19948385550240744, -4.924951120819313743 ) ) ;
#7536 = ORIENTED_EDGE ( 'NONE', *, *, #3228, .F. ) ;
#7537 = EDGE_LOOP ( 'NONE', ( #5963, #4828, #6802, #4776 ) ) ;
#7538 = DIRECTION ( 'NONE',  ( -0.000000000000000000, -0.000000000000000000, 1.000000000000000000 ) ) ;
#7539 = CIRCLE ( 'NONE', #7980, 5.384454397937118664 ) ;
#7540 = LINE ( 'NONE', #335, #231 ) ;
#7541 = CARTESIAN_POINT ( 'NONE',  ( 51.97223112728249816, 50.60051614449765367, -5.992620115222793586 ) ) ;
#7542 = CARTESIAN_POINT ( 'NONE',  ( 42.63976443033212149, 62.00051614449765225, -0.02388180880514948964 ) ) ;
#7543 = CARTESIAN_POINT ( 'NONE',  ( 56.81924384183011512, 46.19948385550240744, 4.924951120819313743 ) ) ;
#7544 = CARTESIAN_POINT ( 'NONE',  ( 4.158806965674306078, 1.986429158307092768, 3.559403772175832259 ) ) ;
#7545 = CARTESIAN_POINT ( 'NONE',  ( 54.72065718078918906, 54.70051614449765509, -6.458785618021089192 ) ) ;
#7546 = CIRCLE ( 'NONE', #11065, 0.7499999999999997780 ) ;
#7547 = AXIS2_PLACEMENT_3D ( 'NONE', #4113, #8337, #9965 ) ;
#7548 = AXIS2_PLACEMENT_3D ( 'NONE', #7514, #9720, #9852 ) ;
#7549 = EDGE_LOOP ( 'NONE', ( #5964, #1703, #5254 ) ) ;
#7550 = EDGE_CURVE ( 'NONE', #13409, #4218, #11055, .T. ) ;
#7551 = VERTEX_POINT ( 'NONE', #5446 ) ;
#7552 = EDGE_CURVE ( 'NONE', #10817, #10955, #7507, .T. ) ;
#7553 = ORIENTED_EDGE ( 'NONE', *, *, #5741, .F. ) ;
#7554 = ORIENTED_EDGE ( 'NONE', *, *, #4598, .T. ) ;
#7555 = CARTESIAN_POINT ( 'NONE',  ( -74.99999999999997158, 20.00000000000001421, 15.00000000000000000 ) ) ;
#7556 = DIRECTION ( 'NONE',  ( -0.000000000000000000, -0.000000000000000000, -1.000000000000000000 ) ) ;
#7557 = ADVANCED_FACE ( 'NONE', ( #10480 ), #1664, .F. ) ;
#7558 = CARTESIAN_POINT ( 'NONE',  ( 2.449293598294706513E-15, -20.00000000000000000, -9.000000000000000000 ) ) ;
#7559 = DIRECTION ( 'NONE',  ( -1.000000000000000000, 0.000000000000000000, 0.000000000000000000 ) ) ;
#7560 = CARTESIAN_POINT ( 'NONE',  ( -62.49999999999997158, 32.50000000000001421, 15.00000000000000000 ) ) ;
#7561 = CIRCLE ( 'NONE', #11075, 1.500000000000001554 ) ;
#7562 = CARTESIAN_POINT ( 'NONE',  ( 53.50833635130540955, 51.69948385550241454, -4.867452303228209765 ) ) ;
#7563 = CARTESIAN_POINT ( 'NONE',  ( 49.97728705011488159, 63.49948385550241170, -7.000000000000000888 ) ) ;
#7564 = CARTESIAN_POINT ( 'NONE',  ( 45.27934281921082516, 47.70051614449766220, 6.458785618021089192 ) ) ;
#7565 = DIRECTION ( 'NONE',  ( -0.000000000000000000, -0.000000000000000000, -1.000000000000000000 ) ) ;
#7566 = CARTESIAN_POINT ( 'NONE',  ( 0.05140428708382657752, 4.819072548984005167, 1.653121499799249605 ) ) ;
#7567 = CARTESIAN_POINT ( 'NONE',  ( 52.25172492374527877, 57.40051614449765083, 7.007379884777203749 ) ) ;
#7568 = CARTESIAN_POINT ( 'NONE',  ( 46.49166364869460466, 56.69948385550240744, 4.867452303228209765 ) ) ;
#7569 = ORIENTED_EDGE ( 'NONE', *, *, #1949, .T. ) ;
#7570 = LINE ( 'NONE', #6600, #11013 ) ;
#7571 = ORIENTED_EDGE ( 'NONE', *, *, #12859, .T. ) ;
#7572 = CARTESIAN_POINT ( 'NONE',  ( 6.385552186430388133, 2.886751345948125991, 4.999999999999999112 ) ) ;
#7573 = VECTOR ( 'NONE', #4516, 1000.000000000000000 ) ;
#7574 = FACE_OUTER_BOUND ( 'NONE', #3976, .T. ) ;
#7575 = CARTESIAN_POINT ( 'NONE',  ( 1.171083334267915221, -24.65495046420793201, 9.999999999999998224 ) ) ;
#7576 =( LENGTH_UNIT ( ) NAMED_UNIT ( * ) SI_UNIT ( .MILLI., .METRE. ) );
#7577 = CARTESIAN_POINT ( 'NONE',  ( 55.96859303347804371, 54.19948385550240033, 4.306917132069425946 ) ) ;
#7578 = AXIS2_PLACEMENT_3D ( 'NONE', #5689, #11765, #9761 ) ;
#7579 = EDGE_CURVE ( 'NONE', #5117, #11058, #8573, .T. ) ;
#7580 = FACE_OUTER_BOUND ( 'NONE', #1264, .T. ) ;
#7581 = CARTESIAN_POINT ( 'NONE',  ( 55.69932041026405045, 51.10051614449766078, 1.875703265242156359 ) ) ;
#7582 = DIRECTION ( 'NONE',  ( -1.000000000000000000, -0.000000000000000000, -0.000000000000000000 ) ) ;
#7583 = CARTESIAN_POINT ( 'NONE',  ( 2.000000000000008882, 3.464101615137749945, 0.000000000000000000 ) ) ;
#7584 = CARTESIAN_POINT ( 'NONE',  ( 6.495567275915080430, -5.834887664329776236, 2.176274696337492837E-17 ) ) ;
#7585 = CARTESIAN_POINT ( 'NONE',  ( 55.94051828345050836, 59.79948385550238754, -4.345558710429104465 ) ) ;
#7586 = AXIS2_PLACEMENT_3D ( 'NONE', #12300, #7200, #10157 ) ;
#7587 = CYLINDRICAL_SURFACE ( 'NONE', #9378, 0.7499999999999997780 ) ;
#7588 = ORIENTED_EDGE ( 'NONE', *, *, #9499, .F. ) ;
#7589 = PRODUCT_DEFINITION_CONTEXT ( 'detailed design', #13418, 'design' ) ;
#7590 = ORIENTED_EDGE ( 'NONE', *, *, #3625, .F. ) ;
#7591 = EDGE_CURVE ( 'NONE', #10020, #12390, #3555, .T. ) ;
#7592 = ADVANCED_FACE ( 'NONE', ( #13013 ), #9524, .T. ) ;
#7593 = EDGE_LOOP ( 'NONE', ( #11464, #3605, #4011, #11812 ) ) ;
#7594 = CARTESIAN_POINT ( 'NONE',  ( -3.453038570459499024, -2.625189405340453419, -3.535263753545272891 ) ) ;
#7595 = CARTESIAN_POINT ( 'NONE',  ( -4.113721387458914807E-15, -4.207632145829740544, 2.712167343862823099 ) ) ;
#7596 = LINE ( 'NONE', #7527, #895 ) ;
#7597 = CARTESIAN_POINT ( 'NONE',  ( 4.175813232069150338, -4.122719923832746325, 2.362127131240695889E-16 ) ) ;
#7598 = CARTESIAN_POINT ( 'NONE',  ( 44.05948171654949874, 52.79948385550240175, 4.345558710429104465 ) ) ;
#7599 = CARTESIAN_POINT ( 'NONE',  ( 43.34962307344078880, 54.10051614449766788, -2.184720259617096705 ) ) ;
#7600 = DIRECTION ( 'NONE',  ( -1.000000000000000000, -0.000000000000000000, -0.000000000000000000 ) ) ;
#7601 = CARTESIAN_POINT ( 'NONE',  ( 43.33558569842703179, 51.09948385550240602, -2.141517661632099223 ) ) ;
#7602 = CARTESIAN_POINT ( 'NONE',  ( 43.18075615816989199, 59.19948385550240744, -4.924951120819313743 ) ) ;
#7603 = AXIS2_PLACEMENT_3D ( 'NONE', #3285, #2104, #9578 ) ;
#7604 = EDGE_LOOP ( 'NONE', ( #11109, #4831, #5421, #5807, #6555 ) ) ;
#7605 = ORIENTED_EDGE ( 'NONE', *, *, #12348, .T. ) ;
#7606 = DIRECTION ( 'NONE',  ( -1.000000000000000000, -0.000000000000000000, -0.000000000000000000 ) ) ;
#7607 = CIRCLE ( 'NONE', #2979, 4.000000000000000000 ) ;
#7608 =( REPRESENTATION_RELATIONSHIP ('NONE','NONE', #5328, #11036 ) REPRESENTATION_RELATIONSHIP_WITH_TRANSFORMATION ( #5159 )SHAPE_REPRESENTATION_RELATIONSHIP( ) );
#7609 = AXIS2_PLACEMENT_3D ( 'NONE', #8967, #7930, #7801 ) ;
#7610 = CARTESIAN_POINT ( 'NONE',  ( 22.00000000000000000, -20.00000000000000000, -12.00000000000000000 ) ) ;
#7611 = CARTESIAN_POINT ( 'NONE',  ( 56.30877334542961421, 57.00051614449766646, 0.02388180880515774693 ) ) ;
#7612 = CARTESIAN_POINT ( 'NONE',  ( 0.1388410611046115850, -3.710337782248037009, -0.5735064479039788665 ) ) ;
#7613 = AXIS2_PLACEMENT_3D ( 'NONE', #6269, #1237, #973 ) ;
#7614 = CARTESIAN_POINT ( 'NONE',  ( 58.41169779390614281, 63.00051614449766646, 0.02388180880515032231 ) ) ;
#7615 = CARTESIAN_POINT ( 'NONE',  ( 4.086262629614028086, 1.979770830881088850, 3.570936333571100629 ) ) ;
#7616 = VECTOR ( 'NONE', #10280, 1000.000000000000000 ) ;
#7617 = CARTESIAN_POINT ( 'NONE',  ( 54.68390685589039890, 57.30051614449767072, 6.485486291978072693 ) ) ;
#7618 = ORIENTED_EDGE ( 'NONE', *, *, #4832, .T. ) ;
#7619 = ORIENTED_EDGE ( 'NONE', *, *, #12159, .T. ) ;
#7620 = ORIENTED_EDGE ( 'NONE', *, *, #9564, .T. ) ;
#7621 = ORIENTED_EDGE ( 'NONE', *, *, #9499, .T. ) ;
#7622 = CIRCLE ( 'NONE', #5632, 4.999999999999999112 ) ;
#7623 = CARTESIAN_POINT ( 'NONE',  ( -62.49999999999997158, 32.50000000000001421, 10.00000000000000000 ) ) ;
#7624 = LINE ( 'NONE', #11828, #5053 ) ;
#7625 = EDGE_CURVE ( 'NONE', #2771, #5545, #11992, .T. ) ;
#7626 = CARTESIAN_POINT ( 'NONE',  ( 2.449293598294706513E-15, -20.00000000000000000, 9.000000000000000000 ) ) ;
#7627 = CYLINDRICAL_SURFACE ( 'NONE', #4350, 15.00000000000000000 ) ;
#7628 = CARTESIAN_POINT ( 'NONE',  ( 46.49166364869460466, 52.69948385550240744, 4.867452303228209765 ) ) ;
#7629 = CARTESIAN_POINT ( 'NONE',  ( 55.94051828345054389, 49.20051614449766220, 4.345558710429044957 ) ) ;
#7630 = ADVANCED_FACE ( 'NONE', ( #9846 ), #2509, .F. ) ;
#7631 = ADVANCED_FACE ( 'NONE', ( #492 ), #258, .F. ) ;
#7632 = CARTESIAN_POINT ( 'NONE',  ( 57.60143344285435774, 49.10051614449766788, 2.493737253992045044 ) ) ;
#7633 = EDGE_CURVE ( 'NONE', #10628, #10472, #13039, .T. ) ;
#7634 = CYLINDRICAL_SURFACE ( 'NONE', #9966, 3.500000000000000000 ) ;
#7635 = DIRECTION ( 'NONE',  ( -0.000000000000000000, -0.000000000000000000, -1.000000000000000000 ) ) ;
#7636 = CARTESIAN_POINT ( 'NONE',  ( 43.34962307344078880, 56.10051614449766078, -2.184720259617096705 ) ) ;
#7637 = CARTESIAN_POINT ( 'NONE',  ( 46.45491332379572924, 63.29948385550240175, -4.840751629271157874 ) ) ;
#7638 = ORIENTED_EDGE ( 'NONE', *, *, #2719, .F. ) ;
#7639 = ADVANCED_FACE ( 'NONE', ( #3422 ), #7710, .T. ) ;
#7640 = DIRECTION ( 'NONE',  ( 1.000000000000000000, 0.000000000000000000, -0.000000000000000000 ) ) ;
#7641 = EDGE_LOOP ( 'NONE', ( #475, #741, #9937, #11617 ) ) ;
#7642 = DIRECTION ( 'NONE',  ( -1.000000000000000000, -0.000000000000000000, -0.000000000000000000 ) ) ;
#7643 = CARTESIAN_POINT ( 'NONE',  ( 0.4465819873852049926, -5.773502691896263528, -3.127607256515468906E-17 ) ) ;
#7644 = CARTESIAN_POINT ( 'NONE',  ( 2.449293598294706513E-15, -20.00000000000000000, 9.000000000000000000 ) ) ;
#7645 = FILL_AREA_STYLE_COLOUR ( '', #11685 ) ;
#7646 = CARTESIAN_POINT ( 'NONE',  ( 55.96859303347804371, 48.19948385550240033, 4.306917132069425946 ) ) ;
#7647 = ADVANCED_FACE ( 'NONE', ( #10875 ), #8748, .F. ) ;
#7648 = EDGE_CURVE ( 'NONE', #9438, #11355, #3791, .T. ) ;
#7649 = CARTESIAN_POINT ( 'NONE',  ( 7.500000000000107470, -32.99038105676652322, -9.000000000000000000 ) ) ;
#7650 = CARTESIAN_POINT ( 'NONE',  ( 53.54508667620424234, 56.70051614449766930, -4.840751629271188961 ) ) ;
#7651 = LINE ( 'NONE', #1129, #9324 ) ;
#7652 = CARTESIAN_POINT ( 'NONE',  ( -12.50000000000000000, 15.00000000000001599, 9.000000000000000000 ) ) ;
#7653 =( LENGTH_UNIT ( ) NAMED_UNIT ( * ) SI_UNIT ( .MILLI., .METRE. ) );
#7654 = CARTESIAN_POINT ( 'NONE',  ( 52.29715082351547295, 58.39948385550238896, 6.992620115222774047 ) ) ;
#7655 = DIRECTION ( 'NONE',  ( 0.000000000000000000, 0.000000000000000000, 1.000000000000000000 ) ) ;
#7656 = VERTEX_POINT ( 'NONE', #10323 ) ;
#7657 = AXIS2_PLACEMENT_3D ( 'NONE', #7985, #700, #9164 ) ;
#7658 = EDGE_LOOP ( 'NONE', ( #10287, #6832, #1942 ) ) ;
#7659 = FACE_OUTER_BOUND ( 'NONE', #6817, .T. ) ;
#7660 = CONICAL_SURFACE ( 'NONE', #7446, 1.535500000000000087, 1.047197551196590748 ) ;
#7661 = DIRECTION ( 'NONE',  ( -0.000000000000000000, -0.000000000000000000, 1.000000000000000000 ) ) ;
#7662 = CARTESIAN_POINT ( 'NONE',  ( 5.000000000000003553, -20.00000000000000000, -8.999999999999998224 ) ) ;
#7663 = CARTESIAN_POINT ( 'NONE',  ( 12.99038105676649835, -12.49999999999984901, -9.000000000000000000 ) ) ;
#7664 = DIRECTION ( 'NONE',  ( -0.04542589977017699732, 0.9989677110047501252, 0.000000000000000000 ) ) ;
#7665 = CARTESIAN_POINT ( 'NONE',  ( 52.25172492374522903, 49.59948385550240602, -7.007379884777227730 ) ) ;
#7666 = CARTESIAN_POINT ( 'NONE',  ( 54.09612160359792199, 51.30051614449766362, 5.676469297603124353 ) ) ;
#7667 = ADVANCED_FACE ( 'NONE', ( #9293 ), #827, .T. ) ;
#7668 = DIRECTION ( 'NONE',  ( -0.000000000000000000, 1.000000000000000000, -0.000000000000000000 ) ) ;
#7669 = CARTESIAN_POINT ( 'NONE',  ( 54.09612160359786515, 49.69948385550240744, -5.676469297603166098 ) ) ;
#7670 = DIRECTION ( 'NONE',  ( -1.000000000000000000, -0.000000000000000000, -0.000000000000000000 ) ) ;
#7671 = CARTESIAN_POINT ( 'NONE',  ( 56.81924384183011512, 64.19948385550240744, 4.924951120819313743 ) ) ;
#7672 = ORIENTED_EDGE ( 'NONE', *, *, #4761, .T. ) ;
#7673 = VERTEX_POINT ( 'NONE', #1813 ) ;
#7674 = VERTEX_POINT ( 'NONE', #694 ) ;
#7675 = CARTESIAN_POINT ( 'NONE',  ( 5.000000000000003553, -20.00000000000000000, 15.00000000000000355 ) ) ;
#7676 = DIRECTION ( 'NONE',  ( 1.000000000000000000, 0.000000000000000000, 0.000000000000000000 ) ) ;
#7677 = CARTESIAN_POINT ( 'NONE',  ( 44.30067958973594955, 54.10051614449766078, -1.875703265242155693 ) ) ;
#7678 = CARTESIAN_POINT ( 'NONE',  ( 49.97728705011495265, 63.50051614449765935, 7.000000000000000888 ) ) ;
#7679 = CARTESIAN_POINT ( 'NONE',  ( 58.41169779390614281, 49.99948385550240459, -0.02388180880523160798 ) ) ;
#7680 = CARTESIAN_POINT ( 'NONE',  ( 49.97728705011488159, 59.49948385550240459, -7.000000000000000888 ) ) ;
#7681 = CARTESIAN_POINT ( 'NONE',  ( 3.974175853610013132, 2.726149789692839054, 2.409821656223150033 ) ) ;
#7682 = CARTESIAN_POINT ( 'NONE',  ( 52.57664461997821093, 61.40051614449765793, 8.007379884777206414 ) ) ;
#7684 = ADVANCED_FACE ( 'NONE', ( #9086 ), #5910, .F. ) ;
#7683 = ORIENTED_EDGE ( 'NONE', *, *, #10131, .T. ) ;
#7685 = ORIENTED_EDGE ( 'NONE', *, *, #1708, .T. ) ;
#7686 = VERTEX_POINT ( 'NONE', #12323 ) ;
#7687 = COLOUR_RGB ( '',0.8941176470588234615, 0.8941176470588234615, 0.8941176470588234615 ) ;
#7688 = EDGE_LOOP ( 'NONE', ( #881, #7995, #12737, #9219 ) ) ;
#7689 = CARTESIAN_POINT ( 'NONE',  ( -9.999999999999994671, 20.00000000000001421, 9.999999999999998224 ) ) ;
#7690 = DIRECTION ( 'NONE',  ( -0.8660254037844373753, 0.5000000000000021094, 0.000000000000000000 ) ) ;
#7691 = ADVANCED_FACE ( 'NONE', ( #13417 ), #13285, .F. ) ;
#7692 = CARTESIAN_POINT ( 'NONE',  ( 4.071447262713887127, 2.020725942163688504, 3.500000000000000000 ) ) ;
#7693 = CARTESIAN_POINT ( 'NONE',  ( 49.97728705011488870, 57.49948385550241170, -6.000000000000000888 ) ) ;
#7694 = CARTESIAN_POINT ( 'NONE',  ( 56.66441430157294690, 46.90051614449765793, -2.141517661632166281 ) ) ;
#7695 = CARTESIAN_POINT ( 'NONE',  ( 41.58830220609386430, 50.00051614449765935, -0.02388180880514929535 ) ) ;
#7696 = CIRCLE ( 'NONE', #12326, 5.000000000000007994 ) ;
#7697 = CARTESIAN_POINT ( 'NONE',  ( 1.925929944387235853E-31, 15.00000000000001599, 15.00000000000000000 ) ) ;
#7698 = CARTESIAN_POINT ( 'NONE',  ( 6.196878017913831194, 3.367876570272813730, -4.166666666666668739 ) ) ;
#7699 = CARTESIAN_POINT ( 'NONE',  ( 49.97728705011495265, 55.50051614449766646, 7.000000000000000888 ) ) ;
#7700 = VECTOR ( 'NONE', #8073, 1000.000000000000227 ) ;
#7701 = EDGE_CURVE ( 'NONE', #9611, #8761, #6673, .T. ) ;
#7702 = EDGE_LOOP ( 'NONE', ( #6330, #8205, #10087, #6709, #6189 ) ) ;
#7703 = FACE_OUTER_BOUND ( 'NONE', #2181, .T. ) ;
#7704 = EDGE_CURVE ( 'NONE', #10628, #2996, #7342, .T. ) ;
#7705 = ORIENTED_EDGE ( 'NONE', *, *, #8983, .F. ) ;
#7706 = DIRECTION ( 'NONE',  ( -0.000000000000000000, -0.000000000000000000, 1.000000000000000000 ) ) ;
#7707 = EDGE_CURVE ( 'NONE', #4538, #3296, #4452, .T. ) ;
#7708 = AXIS2_PLACEMENT_3D ( 'NONE', #2004, #884, #5136 ) ;
#7709 = DIRECTION ( 'NONE',  ( 0.000000000000000000, 0.000000000000000000, 1.000000000000000000 ) ) ;
#7710 = CYLINDRICAL_SURFACE ( 'NONE', #3133, 15.00000000000000000 ) ;
#7711 = VECTOR ( 'NONE', #1204, 1000.000000000000000 ) ;
#7712 = DIRECTION ( 'NONE',  ( 0.000000000000000000, 0.000000000000000000, -1.000000000000000000 ) ) ;
#7713 = CARTESIAN_POINT ( 'NONE',  ( 56.65037692655918988, 59.89948385550241028, -2.184720259617163762 ) ) ;
#7714 = CARTESIAN_POINT ( 'NONE',  ( -6.473970235329672780E-16, -4.862606272033106691, -3.745885042887442395 ) ) ;
#7715 = CARTESIAN_POINT ( 'NONE',  ( 55.71335778527780036, 60.90051614449766504, -1.832500667257213056 ) ) ;
#7716 = DIRECTION ( 'NONE',  ( -0.000000000000000000, -0.000000000000000000, 1.000000000000000000 ) ) ;
#7717 = B_SPLINE_CURVE_WITH_KNOTS ( 'NONE', 3,
 ( #9750, #9877, #7751, #270, #3663 ),
 .UNSPECIFIED., .F., .F.,
 ( 4, 1, 4 ),
 ( 0.000000000000000000, 0.002309401076758506657, 0.004618802153517013315 ),
 .UNSPECIFIED. ) ;
#7718 = DIRECTION ( 'NONE',  ( 1.000000000000000000, 0.000000000000000000, 0.000000000000000000 ) ) ;
#7719 = B_SPLINE_CURVE_WITH_KNOTS ( 'NONE', 3,
 ( #10816, #374, #12951, #5651, #3496, #1333 ),
 .UNSPECIFIED., .F., .F.,
 ( 4, 2, 4 ),
 ( 4.336808689942017736E-19, 0.0002095117440854729585, 0.0004190234881709454834 ),
 .UNSPECIFIED. ) ;
#7720 = CARTESIAN_POINT ( 'NONE',  ( 6.367873360227559232, -5.773502691896263528, 0.000000000000000000 ) ) ;
#7721 = CARTESIAN_POINT ( 'NONE',  ( 43.33558569842703179, 65.09948385550239891, -2.141517661632099223 ) ) ;
#7722 = CARTESIAN_POINT ( 'NONE',  ( 62.50000000000000000, 32.50000000000001421, 15.00000000000000000 ) ) ;
#7723 = ORIENTED_EDGE ( 'NONE', *, *, #2977, .F. ) ;
#7724 = ORIENTED_EDGE ( 'NONE', *, *, #13275, .T. ) ;
#7725 = ORIENTED_EDGE ( 'NONE', *, *, #5860, .T. ) ;
#7726 = CARTESIAN_POINT ( 'NONE',  ( 8.500000000000000000, 2.886751345948125991, 4.999999999999999112 ) ) ;
#7727 = EDGE_CURVE ( 'NONE', #9525, #11021, #7546, .T. ) ;
#7728 = CARTESIAN_POINT ( 'NONE',  ( 0.6640947660595348800, -4.471078309994175548, -3.602146406945708090 ) ) ;
#7729 = PRODUCT_DEFINITION_FORMATION_WITH_SPECIFIED_SOURCE ( 'ANY', '', #3662, .NOT_KNOWN. ) ;
#7730 = CARTESIAN_POINT ( 'NONE',  ( 5.384454397937118664, 0.000000000000000000, -4.484454397937119197 ) ) ;
#7731 = CIRCLE ( 'NONE', #12133, 2.649999999999987477 ) ;
#7732 = CARTESIAN_POINT ( 'NONE',  ( 6.212068001622437663, 3.310128279683251851, 4.266689640018040741 ) ) ;
#7733 = LINE ( 'NONE', #4753, #909 ) ;
#7734 = CARTESIAN_POINT ( 'NONE',  ( 52.25172492374522903, 51.59948385550240602, -7.007379884777227730 ) ) ;
#7735 = CARTESIAN_POINT ( 'NONE',  ( 47.70284917648459100, 53.60051614449765367, 6.992620115222796251 ) ) ;
#7736 = VECTOR ( 'NONE', #6801, 1000.000000000000000 ) ;
#7737 = FACE_OUTER_BOUND ( 'NONE', #4905, .T. ) ;
#7738 = CARTESIAN_POINT ( 'NONE',  ( 52.29715082351547295, 50.39948385550240317, 6.992620115222774047 ) ) ;
#7739 = CARTESIAN_POINT ( 'NONE',  ( 57.36023556966787851, 49.99948385550238328, -0.02388180880522424582 ) ) ;
#7740 = CARTESIAN_POINT ( 'NONE',  ( 43.18075615816989199, 61.19948385550241454, -4.924951120819313743 ) ) ;
#7741 = PRESENTATION_LAYER_ASSIGNMENT (  '', '', ( #1966 ) ) ;
#7742 = AXIS2_PLACEMENT_3D ( 'NONE', #1349, #2461, #8702 ) ;
#7743 = ORIENTED_EDGE ( 'NONE', *, *, #11147, .F. ) ;
#7744 = ORIENTED_EDGE ( 'NONE', *, *, #7807, .T. ) ;
#7745 = DIRECTION ( 'NONE',  ( -3.469446951953614682E-16, 1.000000000000000000, 0.000000000000000000 ) ) ;
#7746 = ORIENTED_EDGE ( 'NONE', *, *, #7292, .T. ) ;
#7747 = CARTESIAN_POINT ( 'NONE',  ( -62.49999999999997158, 20.00000000000001421, -15.00000000000000000 ) ) ;
#7748 = CARTESIAN_POINT ( 'NONE',  ( 8.500000000000000000, -2.886751345948133984, -5.000000000000000000 ) ) ;
#7749 = CARTESIAN_POINT ( 'NONE',  ( 46.45491332379576477, 53.70051614449766220, 4.840751629271188961 ) ) ;
#7750 = CIRCLE ( 'NONE', #13466, 1.500000000000000666 ) ;
#7751 = CARTESIAN_POINT ( 'NONE',  ( -1.999999999999999556, 3.464101615137754830, -3.142992957459232795 ) ) ;
#7752 = CARTESIAN_POINT ( 'NONE',  ( 57.61547081786812896, 50.09948385550240602, 2.450534656007040901 ) ) ;
#7753 = CARTESIAN_POINT ( 'NONE',  ( 55.96859303347804371, 58.19948385550241454, 4.306917132069425946 ) ) ;
#7754 = CARTESIAN_POINT ( 'NONE',  ( 62.49999999999998579, 0.000000000000000000, -9.999999999999998224 ) ) ;
#7755 = CARTESIAN_POINT ( 'NONE',  ( 49.97728705011495265, 61.50051614449766646, 8.000000000000001776 ) ) ;
#7756 = ORIENTED_EDGE ( 'NONE', *, *, #4500, .F. ) ;
#7757 = AXIS2_PLACEMENT_3D ( 'NONE', #2306, #5504, #3286 ) ;
#7758 = EDGE_LOOP ( 'NONE', ( #7238, #1788, #8223 ) ) ;
#7759 = VERTEX_POINT ( 'NONE', #7227 ) ;
#7760 = ORIENTED_EDGE ( 'NONE', *, *, #7251, .T. ) ;
#7761 = LINE ( 'NONE', #5484, #10508 ) ;
#7762 = CARTESIAN_POINT ( 'NONE',  ( -4.999999999999998224, -20.00000000000000000, 15.00000000000000355 ) ) ;
#7763 = DIRECTION ( 'NONE',  ( -1.000000000000000000, 0.000000000000000000, 0.000000000000000000 ) ) ;
#7764 =( LENGTH_UNIT ( ) NAMED_UNIT ( * ) SI_UNIT ( .MILLI., .METRE. ) );
#7765 = CARTESIAN_POINT ( 'NONE',  ( 44.30067958973596376, 54.89948385550240317, 1.875703265242204099 ) ) ;
#7766 = CARTESIAN_POINT ( 'NONE',  ( 44.03140696652198471, 49.80051614449765651, 4.306917132069485454 ) ) ;
#7767 = CARTESIAN_POINT ( 'NONE',  ( 52.57664461997821093, 53.40051614449765793, 8.007379884777206414 ) ) ;
#7768 = VECTOR ( 'NONE', #10041, 1000.000000000000000 ) ;
#7769 = ADVANCED_FACE ( 'NONE', ( #11150 ), #8190, .T. ) ;
#7770 = CARTESIAN_POINT ( 'NONE',  ( 7.336184427528458230, 9.926022037524705097E-16, 8.105212085995399107 ) ) ;
#7771 = CIRCLE ( 'NONE', #9534, 7.900000000000002132 ) ;
#7772 = CARTESIAN_POINT ( 'NONE',  ( 53.93078149122418807, 45.00000000000000000, -5.235029531081472953 ) ) ;
#7773 = CARTESIAN_POINT ( 'NONE',  ( 44.05948171654945611, 64.20051614449765509, -4.345558710429044069 ) ) ;
#7774 = ORIENTED_EDGE ( 'NONE', *, *, #2577, .F. ) ;
#7775 = DIRECTION ( 'NONE',  ( 4.082155997157843695E-16, -1.000000000000000000, 0.000000000000000000 ) ) ;
#7776 = ORIENTED_EDGE ( 'NONE', *, *, #8130, .T. ) ;
#7777 = CARTESIAN_POINT ( 'NONE',  ( 12.50000000000000000, 15.00000000000001776, 9.000000000000000000 ) ) ;
#7778 = PRODUCT ( 'driver roller', 'driver roller', '', ( #11218 ) ) ;
#7779 = FACE_OUTER_BOUND ( 'NONE', #13431, .T. ) ;
#7780 = CIRCLE ( 'NONE', #1804, 5.200000000000001066 ) ;
#7781 = CARTESIAN_POINT ( 'NONE',  ( 0.000000000000000000, 0.000000000000000000, -4.000000000000000000 ) ) ;
#7782 = DIRECTION ( 'NONE',  ( 0.000000000000000000, 0.000000000000000000, 1.000000000000000000 ) ) ;
#7783 = CARTESIAN_POINT ( 'NONE',  ( 45.90387839640214196, 56.69948385550240744, 5.676469297603166098 ) ) ;
#7784 = CARTESIAN_POINT ( 'NONE',  ( 56.30877334542961421, 59.00051614449766646, 0.02388180880515774693 ) ) ;
#7785 = CARTESIAN_POINT ( 'NONE',  ( -59.84999999999998721, 32.50000000000001421, 15.00000000000000000 ) ) ;
#7786 = CARTESIAN_POINT ( 'NONE',  ( 6.534838248920897819, 2.951765777552412651, 5.112608298763836601 ) ) ;
#7787 = CARTESIAN_POINT ( 'NONE',  ( 56.65037692655921120, 45.10051614449766078, 2.184720259617097593 ) ) ;
#7788 = CARTESIAN_POINT ( 'NONE',  ( 45.86712807150323812, 65.29948385550241596, -5.649768623646098220 ) ) ;
#7789 = VECTOR ( 'NONE', #2700, 1000.000000000000000 ) ;
#7790 = CARTESIAN_POINT ( 'NONE',  ( 20.00000000000000000, -25.00000000000000711, -23.00000000000000000 ) ) ;
#7791 = EDGE_LOOP ( 'NONE', ( #2232, #6055, #808 ) ) ;
#7792 = ORIENTED_EDGE ( 'NONE', *, *, #1116, .T. ) ;
#7793 =( REPRESENTATION_RELATIONSHIP ('NONE','NONE', #5328, #7264 ) REPRESENTATION_RELATIONSHIP_WITH_TRANSFORMATION ( #2487 )SHAPE_REPRESENTATION_RELATIONSHIP( ) );
#7794 = VECTOR ( 'NONE', #5344, 1000.000000000000000 ) ;
#7795 = EDGE_CURVE ( 'NONE', #1508, #3673, #6883, .T. ) ;
#7796 = EDGE_LOOP ( 'NONE', ( #9084, #12438, #12404, #2083, #1700, #9133 ) ) ;
#7797 = CYLINDRICAL_SURFACE ( 'NONE', #7038, 1.999999999999998224 ) ;
#7798 = CARTESIAN_POINT ( 'NONE',  ( 4.197393957002303999, -0.4069871074557456780, -3.503767560748925813 ) ) ;
#7799 = LINE ( 'NONE', #4613, #13257 ) ;
#7800 = CARTESIAN_POINT ( 'NONE',  ( -74.99999999999998579, 7.499999999999975131, -10.00000000000000000 ) ) ;
#7801 = DIRECTION ( 'NONE',  ( 0.000000000000000000, 1.000000000000000000, 0.000000000000000000 ) ) ;
#7802 = CIRCLE ( 'NONE', #9563, 2.100000000000000089 ) ;
#7803 = CARTESIAN_POINT ( 'NONE',  ( 57.36023556966787851, 53.00051614449765225, 0.02388180880515038476 ) ) ;
#7804 = DIRECTION ( 'NONE',  ( -0.000000000000000000, -0.000000000000000000, -1.000000000000000000 ) ) ;
#7805 = CARTESIAN_POINT ( 'NONE',  ( 56.66441430157296821, 54.09948385550240602, 2.141517661632100111 ) ) ;
#7806 = EDGE_CURVE ( 'NONE', #6754, #7186, #4945, .T. ) ;
#7807 = EDGE_CURVE ( 'NONE', #2711, #3301, #6247, .T. ) ;
#7808 = CARTESIAN_POINT ( 'NONE',  ( 43.18075615816989199, 65.19948385550240744, -4.924951120819313743 ) ) ;
#7809 = CIRCLE ( 'NONE', #1831, 12.50000000000000000 ) ;
#7810 = ORIENTED_EDGE ( 'NONE', *, *, #12682, .F. ) ;
#7811 = ORIENTED_EDGE ( 'NONE', *, *, #7218, .F. ) ;
#7812 = DIRECTION ( 'NONE',  ( -4.082155997157844188E-16, 1.000000000000000000, 0.000000000000000000 ) ) ;
#7813 = ORIENTED_EDGE ( 'NONE', *, *, #13535, .T. ) ;
#7814 = DIRECTION ( 'NONE',  ( 1.000000000000000000, 0.000000000000000000, -0.000000000000000000 ) ) ;
#7815 = CARTESIAN_POINT ( 'NONE',  ( 1.734723475976807094E-15, 4.618802153517012954, -0.4999999999999995559 ) ) ;
#7816 = CARTESIAN_POINT ( 'NONE',  ( 55.08986747509849380, 57.20051614449766220, 3.727524721679155384 ) ) ;
#7817 = DIRECTION ( 'NONE',  ( -0.8660254037844412611, 0.4999999999999956146, 0.000000000000000000 ) ) ;
#7818 = CARTESIAN_POINT ( 'NONE',  ( 56.81924384183011512, 52.19948385550240744, 4.924951120819313743 ) ) ;
#7819 = EDGE_CURVE ( 'NONE', #4149, #822, #9011, .T. ) ;
#7820 = CARTESIAN_POINT ( 'NONE',  ( 54.13287192849676188, 54.29948385550240886, 5.649768623646098220 ) ) ;
#7821 = CARTESIAN_POINT ( 'NONE',  ( 0.000000000000000000, 3.031088913245533867, 1.750000000000002887 ) ) ;
#7822 = AXIS2_PLACEMENT_3D ( 'NONE', #11448, #10410, #6001 ) ;
#7823 = CARTESIAN_POINT ( 'NONE',  ( 57.60143344285435774, 61.10051614449766788, 2.493737253992045044 ) ) ;
#7824 = ORIENTED_EDGE ( 'NONE', *, *, #6449, .F. ) ;
#7825 = EDGE_LOOP ( 'NONE', ( #10217, #3827, #1859, #6918 ) ) ;
#7826 = VERTEX_POINT ( 'NONE', #4872 ) ;
#7827 = ORIENTED_EDGE ( 'NONE', *, *, #12563, .F. ) ;
#7828 = EDGE_CURVE ( 'NONE', #2854, #13025, #5131, .T. ) ;
#7829 = CYLINDRICAL_SURFACE ( 'NONE', #348, 15.00000000000000000 ) ;
#7830 = SURFACE_STYLE_USAGE ( .BOTH. , #5485 ) ;
#7832 = AXIS2_PLACEMENT_3D ( 'NONE', #4525, #12192, #3554 ) ;
#7831 =( NAMED_UNIT ( * ) SI_UNIT ( $, .STERADIAN. ) SOLID_ANGLE_UNIT ( ) );
#7833 = CARTESIAN_POINT ( 'NONE',  ( -62.49999999999997158, 32.50000000000001421, 9.999999999999998224 ) ) ;
#7834 = LINE ( 'NONE', #5692, #9860 ) ;
#7835 = CARTESIAN_POINT ( 'NONE',  ( 56.30877334542961421, 55.99948385550241170, -0.02388180880520959434 ) ) ;
#7836 = CARTESIAN_POINT ( 'NONE',  ( 44.05948171654945611, 46.20051614449766220, -4.345558710429044069 ) ) ;
#7837 = AXIS2_PLACEMENT_3D ( 'NONE', #12269, #3837, #4809 ) ;
#7838 = CARTESIAN_POINT ( 'NONE',  ( 49.97728705011495265, 51.50051614449765935, 8.000000000000001776 ) ) ;
#7839 = FACE_OUTER_BOUND ( 'NONE', #13450, .T. ) ;
#7840 = DIRECTION ( 'NONE',  ( 0.000000000000000000, 0.000000000000000000, -1.000000000000000000 ) ) ;
#7841 = AXIS2_PLACEMENT_3D ( 'NONE', #12830, #11802, #11664 ) ;
#7842 = CARTESIAN_POINT ( 'NONE',  ( 50.02271294988505446, 44.50051614449765935, -8.000000000000001776 ) ) ;
#7843 = AXIS2_PLACEMENT_3D ( 'NONE', #6710, #7606, #1083 ) ;
#7844 = ORIENTED_EDGE ( 'NONE', *, *, #10834, .T. ) ;
#7845 = CARTESIAN_POINT ( 'NONE',  ( -0.3461262719736137305, 4.658553426539289610, -3.671615880910373608 ) ) ;
#7846 = VERTEX_POINT ( 'NONE', #9156 ) ;
#7847 = DIRECTION ( 'NONE',  ( 1.000000000000000000, 0.000000000000000000, 0.000000000000000000 ) ) ;
#7848 = CARTESIAN_POINT ( 'NONE',  ( 3.961551342853212532, -2.319461885623237851, -2.982574167881048677 ) ) ;
#7849 = DIRECTION ( 'NONE',  ( 1.000000000000000000, 0.000000000000000000, 0.000000000000000000 ) ) ;
#7850 = CARTESIAN_POINT ( 'NONE',  ( 57.36023556966787851, 57.99948385550239038, -0.02388180880522424582 ) ) ;
#7851 = CIRCLE ( 'NONE', #3622, 12.49999999999999645 ) ;
#7852 = CARTESIAN_POINT ( 'NONE',  ( 55.71335778527780036, 56.90051614449767214, -1.832500667257213056 ) ) ;
#7853 = CARTESIAN_POINT ( 'NONE',  ( -5.560781378645575757, 6.809993116116508640E-16, -4.000000000000000000 ) ) ;
#7854 = CARTESIAN_POINT ( 'NONE',  ( 2.344047193898588954, 3.265465875126468021, -5.031375706690542042E-16 ) ) ;
#7855 = CARTESIAN_POINT ( 'NONE',  ( 49.97728705011495265, 45.50051614449765935, 7.000000000000000888 ) ) ;
#7856 = CARTESIAN_POINT ( 'NONE',  ( 48.07319477248768180, 48.59948385550239891, 6.007379884777225953 ) ) ;
#7857 = CARTESIAN_POINT ( 'NONE',  ( -62.49999999999997158, 32.50000000000001421, 15.00000000000000178 ) ) ;
#7858 = ORIENTED_EDGE ( 'NONE', *, *, #4090, .T. ) ;
#7859 = UNCERTAINTY_MEASURE_WITH_UNIT (LENGTH_MEASURE( 1.000000000000000082E-05 ), #1906, 'distance_accuracy_value', 'NONE');
#7860 = ORIENTED_EDGE ( 'NONE', *, *, #1158, .T. ) ;
#7861 = CARTESIAN_POINT ( 'NONE',  ( 3.098410542199072637, -7.060458129626440815, 0.000000000000000000 ) ) ;
#7862 = PRODUCT_DEFINITION_SHAPE ( 'NONE', 'NONE',  #11484 ) ;
#7863 = CARTESIAN_POINT ( 'NONE',  ( 4.198928548860774157, -0.8158838809860124996, -3.526471437616918170 ) ) ;
#7864 = CARTESIAN_POINT ( 'NONE',  ( 6.367873360227555679, -2.886751345948119774, 4.999999999999999112 ) ) ;
#7865 =( NAMED_UNIT ( * ) PLANE_ANGLE_UNIT ( ) SI_UNIT ( $, .RADIAN. ) );
#7866 = CARTESIAN_POINT ( 'NONE',  ( 1.498123826657866475, -5.075000000000000178, 0.000000000000000000 ) ) ;
#7867 = CARTESIAN_POINT ( 'NONE',  ( 53.50000000000000000, 0.000000000000000000, 0.000000000000000000 ) ) ;
#7868 = ADVANCED_FACE ( 'NONE', ( #11217 ), #12259, .F. ) ;
#7869 = CARTESIAN_POINT ( 'NONE',  ( 43.33558569842706021, 53.90051614449765793, 2.141517661632167169 ) ) ;
#7870 = CARTESIAN_POINT ( 'NONE',  ( 6.207660606243411650, -2.016205878028328957, -5.000000000000000000 ) ) ;
#7871 = LINE ( 'NONE', #5935, #7616 ) ;
#7872 = CARTESIAN_POINT ( 'NONE',  ( 43.33558569842703179, 55.09948385550241312, -2.141517661632099223 ) ) ;
#7873 = CARTESIAN_POINT ( 'NONE',  ( 52.25172492374522903, 47.59948385550239891, -7.007379884777225953 ) ) ;
#7874 = AXIS2_PLACEMENT_3D ( 'NONE', #6747, #13215, #13289 ) ;
#7875 = CARTESIAN_POINT ( 'NONE',  ( 49.97728705011486738, 61.49948385550241170, -8.000000000000001776 ) ) ;
#7876 = EDGE_CURVE ( 'NONE', #10143, #3623, #4673, .T. ) ;
#7877 = VERTEX_POINT ( 'NONE', #4308 ) ;
#7878 = EDGE_LOOP ( 'NONE', ( #11301, #10334, #279, #9883, #2417, #1318, #12494 ) ) ;
#7879 = CARTESIAN_POINT ( 'NONE',  ( 4.158807179406255550, 2.089320655794525639, -3.500000000000000000 ) ) ;
#7880 = EDGE_CURVE ( 'NONE', #11165, #3637, #3204, .T. ) ;
#7881 = ORIENTED_EDGE ( 'NONE', *, *, #9481, .F. ) ;
#7882 = EDGE_CURVE ( 'NONE', #6095, #4029, #1594, .T. ) ;
#7883 = CARTESIAN_POINT ( 'NONE',  ( 0.000000000000000000, 0.000000000000000000, 0.000000000000000000 ) ) ;
#7884 = EDGE_CURVE ( 'NONE', #12293, #2807, #10528, .T. ) ;
#7885 = DIRECTION ( 'NONE',  ( 1.000000000000000000, 0.000000000000000000, 0.000000000000000000 ) ) ;
#7886 = CARTESIAN_POINT ( 'NONE',  ( 49.97728705011494554, 57.50051614449766646, 6.000000000000000888 ) ) ;
#7887 = CARTESIAN_POINT ( 'NONE',  ( 47.70284917648459810, 63.60051614449766078, 6.992620115222797139 ) ) ;
#7888 = CARTESIAN_POINT ( 'NONE',  ( 57.60143344285433642, 53.89948385550240317, -2.493737253992118319 ) ) ;
#7889 = CARTESIAN_POINT ( 'NONE',  ( 54.09612160359786515, 57.69948385550240744, -5.676469297603166098 ) ) ;
#7890 = DIRECTION ( 'NONE',  ( -1.000000000000000000, 0.000000000000000000, 0.000000000000000000 ) ) ;
#7891 = CARTESIAN_POINT ( 'NONE',  ( 52.62207051974839089, 46.39948385550240317, 7.992620115222770494 ) ) ;
#7892 = ORIENTED_EDGE ( 'NONE', *, *, #8540, .T. ) ;
#7893 = ORIENTED_EDGE ( 'NONE', *, *, #7051, .T. ) ;
#7894 = EDGE_LOOP ( 'NONE', ( #10957, #8491, #3805 ) ) ;
#7895 = ORIENTED_EDGE ( 'NONE', *, *, #8130, .F. ) ;
#7896 = AXIS2_PLACEMENT_3D ( 'NONE', #7153, #6394, #7223 ) ;
#7897 = DIRECTION ( 'NONE',  ( 0.000000000000000000, 0.000000000000000000, 1.000000000000000000 ) ) ;
#7898 = FILL_AREA_STYLE ('',( #11829 ) ) ;
#7899 = CARTESIAN_POINT ( 'NONE',  ( 1.267864665251833278E-11, -20.00000000000000000, 9.000000000000000000 ) ) ;
#7900 = FACE_OUTER_BOUND ( 'NONE', #2037, .T. ) ;
#7901 = CARTESIAN_POINT ( 'NONE',  ( 55.08986747509847248, 57.79948385550240175, -3.727524721679197572 ) ) ;
#7902 = CARTESIAN_POINT ( 'NONE',  ( 54.13287192849671214, 48.70051614449766220, -5.649768623646139964 ) ) ;
#7903 = CARTESIAN_POINT ( 'NONE',  ( 47.42335538002180328, 52.40051614449767214, -8.007379884777206414 ) ) ;
#7904 = CYLINDRICAL_SURFACE ( 'NONE', #9323, 1.500000000000001332 ) ;
#7905 = LINE ( 'NONE', #12186, #3375 ) ;
#7906 = CARTESIAN_POINT ( 'NONE',  ( 55.94051828345053679, 61.20051614449766220, 4.345558710429044069 ) ) ;
#7907 = VERTEX_POINT ( 'NONE', #9627 ) ;
#7908 = DIRECTION ( 'NONE',  ( -0.000000000000000000, -0.000000000000000000, -1.000000000000000000 ) ) ;
#7909 = VERTEX_POINT ( 'NONE', #16 ) ;
#7910 = EDGE_CURVE ( 'NONE', #6904, #7909, #12182, .T. ) ;
#7911 = CARTESIAN_POINT ( 'NONE',  ( -2.649999999999988809, 15.00000000000001599, -15.00000000000000000 ) ) ;
#7912 = CARTESIAN_POINT ( 'NONE',  ( 4.180345304246199767, -4.135116856707399258, 0.02129519942689610257 ) ) ;
#7913 = DIRECTION ( 'NONE',  ( 0.000000000000000000, -1.000000000000000000, 0.000000000000000000 ) ) ;
#7914 = CARTESIAN_POINT ( 'NONE',  ( 56.65037692655918988, 55.89948385550240317, -2.184720259617163762 ) ) ;
#7915 = AXIS2_PLACEMENT_3D ( 'NONE', #12858, #217, #4436 ) ;
#7916 = CARTESIAN_POINT ( 'NONE',  ( 46.49166364869456913, 58.30051614449765651, -4.867452303228181343 ) ) ;
#7917 = CYLINDRICAL_SURFACE ( 'NONE', #6556, 5.000000000000000888 ) ;
#7918 = DIRECTION ( 'NONE',  ( 1.000000000000000000, 0.000000000000000000, -0.000000000000000000 ) ) ;
#7919 = CARTESIAN_POINT ( 'NONE',  ( 44.88205777487401349, 61.80051614449766362, 3.688883143319584779 ) ) ;
#7920 = CARTESIAN_POINT ( 'NONE',  ( 49.97728705011488159, 63.49948385550241170, -7.000000000000000888 ) ) ;
#7921 = CARTESIAN_POINT ( 'NONE',  ( -62.49999999999997158, 32.50000000000001421, 15.00000000000000000 ) ) ;
#7922 = VERTEX_POINT ( 'NONE', #2219 ) ;
#7923 = CIRCLE ( 'NONE', #10996, 12.49999999999999645 ) ;
#7924 = ORIENTED_EDGE ( 'NONE', *, *, #13033, .T. ) ;
#7925 = CARTESIAN_POINT ( 'NONE',  ( 2.449293598294706513E-15, -20.00000000000000000, 15.00000000000000355 ) ) ;
#7926 = CARTESIAN_POINT ( 'NONE',  ( 4.197393957002303999, 7.772902908466098641E-14, -3.503767560748929810 ) ) ;
#7927 = CARTESIAN_POINT ( 'NONE',  ( 4.158921614371307918, -1.986121848748762186, 3.559936047944509241 ) ) ;
#7928 = SURFACE_STYLE_USAGE ( .BOTH. , #8834 ) ;
#7929 = CARTESIAN_POINT ( 'NONE',  ( 5.599999999999999645, 0.000000000000000000, 0.000000000000000000 ) ) ;
#7930 = DIRECTION ( 'NONE',  ( 1.000000000000000000, 3.469446951953615175E-16, 0.000000000000000000 ) ) ;
#7931 = CARTESIAN_POINT ( 'NONE',  ( 47.70284917648459100, 57.60051614449764656, 6.992620115222796251 ) ) ;
#7932 = AXIS2_PLACEMENT_3D ( 'NONE', #2839, #11913, #9066 ) ;
#7933 = CARTESIAN_POINT ( 'NONE',  ( 10.00000000000000000, 25.00000000000001776, -15.00000000000000000 ) ) ;
#7934 = CARTESIAN_POINT ( 'NONE',  ( 0.000000000000000000, 40.00000000000001421, 9.999999999999998224 ) ) ;
#7935 = CARTESIAN_POINT ( 'NONE',  ( 47.70284917648453415, 55.39948385550238896, -6.992620115222774047 ) ) ;
#7936 = CARTESIAN_POINT ( 'NONE',  ( 44.05948171654949874, 46.79948385550238754, 4.345558710429105354 ) ) ;
#7937 = VECTOR ( 'NONE', #12738, 1000.000000000000000 ) ;
#7938 = CARTESIAN_POINT ( 'NONE',  ( 43.18075615816989199, 63.19948385550240744, -4.924951120819313743 ) ) ;
#7939 = ADVANCED_FACE ( 'NONE', ( #7429 ), #7490, .T. ) ;
#7940 = EDGE_LOOP ( 'NONE', ( #4121, #1100, #9940, #9186 ) ) ;
#7941 = EDGE_LOOP ( 'NONE', ( #7133, #5029, #9639, #9343, #4448, #5150, #2050, #8933 ) ) ;
#7942 =( GEOMETRIC_REPRESENTATION_CONTEXT ( 3 ) GLOBAL_UNCERTAINTY_ASSIGNED_CONTEXT ( ( #5791 ) ) GLOBAL_UNIT_ASSIGNED_CONTEXT ( ( #4751, #10057, #1477 ) ) REPRESENTATION_CONTEXT ( 'NONE', 'WORKASPACE' ) );
#7943 = DIRECTION ( 'NONE',  ( 0.000000000000000000, 0.000000000000000000, 1.000000000000000000 ) ) ;
#7944 = CONICAL_SURFACE ( 'NONE', #1296, 5.000000000000000000, 1.047197551196600296 ) ;
#7945 = EDGE_LOOP ( 'NONE', ( #5046, #1644, #2852, #880 ) ) ;
#7946 = FACE_BOUND ( 'NONE', #9409, .T. ) ;
#7947 = CARTESIAN_POINT ( 'NONE',  ( 6.466260427357664042, -2.904280683598015500, -5.030361703432624232 ) ) ;
#7948 = CARTESIAN_POINT ( 'NONE',  ( 53.54508667620424234, 62.70051614449766220, -4.840751629271188961 ) ) ;
#7949 = CARTESIAN_POINT ( 'NONE',  ( 0.2182387239012630320, 1.693823289460900883, -3.499999999999999112 ) ) ;
#7950 = CARTESIAN_POINT ( 'NONE',  ( 43.18075615816989199, 65.19948385550240744, -4.924951120819313743 ) ) ;
#7951 = CARTESIAN_POINT ( 'NONE',  ( 43.18075615816989199, 51.19948385550240744, -4.924951120819313743 ) ) ;
#7952 = VECTOR ( 'NONE', #5933, 1000.000000000000000 ) ;
#7953 = CARTESIAN_POINT ( 'NONE',  ( 50.02271294988512551, 64.49948385550240459, 7.000000000000000888 ) ) ;
#7954 = DIRECTION ( 'NONE',  ( -1.000000000000000000, 0.000000000000000000, 0.000000000000000000 ) ) ;
#7955 = CARTESIAN_POINT ( 'NONE',  ( 42.38452918213190657, 61.90051614449766504, 2.450534656007115508 ) ) ;
#7956 = ORIENTED_EDGE ( 'NONE', *, *, #4540, .T. ) ;
#7957 = ORIENTED_EDGE ( 'NONE', *, *, #8609, .T. ) ;
#7958 = ORIENTED_EDGE ( 'NONE', *, *, #11285, .T. ) ;
#7959 = ORIENTED_EDGE ( 'NONE', *, *, #2973, .T. ) ;
#7960 = PRESENTATION_LAYER_ASSIGNMENT (  '', '', ( #648 ) ) ;
#7961 = DIRECTION ( 'NONE',  ( 0.000000000000000000, 0.000000000000000000, 1.000000000000000000 ) ) ;
#7962 = VECTOR ( 'NONE', #13066, 1000.000000000000000 ) ;
#7963 = FACE_OUTER_BOUND ( 'NONE', #780, .T. ) ;
#7964 = DIRECTION ( 'NONE',  ( -0.000000000000000000, -0.000000000000000000, -1.000000000000000000 ) ) ;
#7965 = LINE ( 'NONE', #4998, #558 ) ;
#7966 = CARTESIAN_POINT ( 'NONE',  ( 44.28664221472220675, 63.09948385550240602, -1.832500667257165317 ) ) ;
#7967 = CARTESIAN_POINT ( 'NONE',  ( 57.36023556966787851, 55.00051614449765935, 0.02388180880515038476 ) ) ;
#7968 = CARTESIAN_POINT ( 'NONE',  ( 57.61547081786810764, 54.90051614449765793, -2.450534656007114176 ) ) ;
#7969 = DIRECTION ( 'NONE',  ( 1.000000000000000000, 3.469446951953615668E-16, -0.000000000000000000 ) ) ;
#7970 = EDGE_CURVE ( 'NONE', #5544, #12042, #10357, .T. ) ;
#7971 = CARTESIAN_POINT ( 'NONE',  ( 57.60143344285435774, 45.10051614449766788, 2.493737253992045044 ) ) ;
#7972 = EDGE_CURVE ( 'NONE', #2821, #1050, #5346, .T. ) ;
#7973 = AXIS2_PLACEMENT_3D ( 'NONE', #2127, #127, #4348 ) ;
#7974 = VERTEX_POINT ( 'NONE', #5158 ) ;
#7975 = CARTESIAN_POINT ( 'NONE',  ( 1.828356344711641102, 3.563200125723180900, -5.433716356636336675E-16 ) ) ;
#7976 = ADVANCED_FACE ( 'NONE', ( #8459, #1176 ), #9561, .T. ) ;
#7977 = ORIENTED_EDGE ( 'NONE', *, *, #8218, .F. ) ;
#7978 = LINE ( 'NONE', #13012, #3403 ) ;
#7979 = CARTESIAN_POINT ( 'NONE',  ( -59.84999999999998721, 32.50000000000001421, 15.00000000000000000 ) ) ;
#7980 = AXIS2_PLACEMENT_3D ( 'NONE', #1006, #6302, #10496 ) ;
#7981 = DIRECTION ( 'NONE',  ( -0.7779254092217071648, -0.6283566325640552730, 1.130512422757410501E-16 ) ) ;
#7982 = CARTESIAN_POINT ( 'NONE',  ( 52.29715082351547295, 58.39948385550238896, 6.992620115222774047 ) ) ;
#7983 = CARTESIAN_POINT ( 'NONE',  ( 47.74827507625477807, 52.59948385550239891, 7.007379884777229506 ) ) ;
#7984 = DIRECTION ( 'NONE',  ( 0.000000000000000000, 0.000000000000000000, 1.000000000000000000 ) ) ;
#7985 = CARTESIAN_POINT ( 'NONE',  ( 0.000000000000000000, 0.000000000000000000, -5.000000000000000888 ) ) ;
#7986 = DIRECTION ( 'NONE',  ( -0.000000000000000000, 1.000000000000000000, -0.000000000000000000 ) ) ;
#7987 = CARTESIAN_POINT ( 'NONE',  ( 55.96859303347802239, 44.80051614449767072, -4.306917132069484566 ) ) ;
#7988 = CARTESIAN_POINT ( 'NONE',  ( 44.28664221472220675, 49.09948385550241312, -1.832500667257165317 ) ) ;
#7989 = CARTESIAN_POINT ( 'NONE',  ( 2.000000000000000000, -0.8865213383406730374, -1.535499999999999421 ) ) ;
#7990 = ORIENTED_EDGE ( 'NONE', *, *, #9483, .F. ) ;
#7991 = AXIS2_PLACEMENT_3D ( 'NONE', #3132, #11696, #10598 ) ;
#7992 = AXIS2_PLACEMENT_3D ( 'NONE', #3037, #12505, #7266 ) ;
#7993 = AXIS2_PLACEMENT_3D ( 'NONE', #13164, #2668, #2528 ) ;
#7994 = VERTEX_POINT ( 'NONE', #3336 ) ;
#7995 = ORIENTED_EDGE ( 'NONE', *, *, #846, .T. ) ;
#7996 = FACE_OUTER_BOUND ( 'NONE', #1436, .T. ) ;
#7997 = CARTESIAN_POINT ( 'NONE',  ( 0.000000000000000000, 0.000000000000000000, -3.499999999999999556 ) ) ;
#7998 = CARTESIAN_POINT ( 'NONE',  ( 6.357976367241527704, -5.421935536068480666, -0.8264656814046078548 ) ) ;
#7999 = FILL_AREA_STYLE_COLOUR ( '', #6612 ) ;
#8000 = CARTESIAN_POINT ( 'NONE',  ( 6.541334219041338827, 5.921300567812616933, -0.03049376373817709943 ) ) ;
#8001 = CARTESIAN_POINT ( 'NONE',  ( 4.093692494532773729, -2.021783646005766766, 3.501831996793844493 ) ) ;
#8002 = CARTESIAN_POINT ( 'NONE',  ( 56.65037692655921120, 57.10051614449766078, 2.184720259617097593 ) ) ;
#8003 = CARTESIAN_POINT ( 'NONE',  ( 0.2499999999999966416, -8.096141056083448362, -1.000000000000000000 ) ) ;
#8004 = CARTESIAN_POINT ( 'NONE',  ( 46.45491332379572924, 65.29948385550241596, -4.840751629271157874 ) ) ;
#8005 = LINE ( 'NONE', #859, #1634 ) ;
#8006 = CARTESIAN_POINT ( 'NONE',  ( 42.63976443033212860, 58.99948385550239038, 0.02388180880522514787 ) ) ;
#8007 = CARTESIAN_POINT ( 'NONE',  ( 52.25172492374522903, 49.59948385550240602, -7.007379884777225953 ) ) ;
#8008 = ADVANCED_FACE ( 'NONE', ( #12602, #5428 ), #9364, .T. ) ;
#8009 = CARTESIAN_POINT ( 'NONE',  ( 45.90387839640214196, 48.69948385550240744, 5.676469297603166098 ) ) ;
#8010 = ORIENTED_EDGE ( 'NONE', *, *, #4647, .F. ) ;
#8011 = ORIENTED_EDGE ( 'NONE', *, *, #13238, .F. ) ;
#8012 = CARTESIAN_POINT ( 'NONE',  ( -18.00000000000000355, -19.99999999999999289, -12.00000000000000000 ) ) ;
#8013 = ORIENTED_EDGE ( 'NONE', *, *, #6713, .T. ) ;
#8014 = CARTESIAN_POINT ( 'NONE',  ( 0.2175679805369682140, -1.691499766289324080, 3.500000000000000000 ) ) ;
#8015 = CIRCLE ( 'NONE', #2049, 4.000000000000003553 ) ;
#8016 = CARTESIAN_POINT ( 'NONE',  ( 6.534224484704326485, -2.950930484791631780, -5.111161529262894909 ) ) ;
#8017 = CARTESIAN_POINT ( 'NONE',  ( 49.97728705011494554, 61.50051614449766646, 6.000000000000000888 ) ) ;
#8018 = AXIS2_PLACEMENT_3D ( 'NONE', #11898, #9830, #349 ) ;
#8019 = FACE_OUTER_BOUND ( 'NONE', #1574, .T. ) ;
#8020 = CARTESIAN_POINT ( 'NONE',  ( 54.72065718078924590, 58.29948385550240886, 6.458785618021043895 ) ) ;
#8021 = CARTESIAN_POINT ( 'NONE',  ( 45.86712807150323812, 61.29948385550240886, -5.649768623646098220 ) ) ;
#8022 = CARTESIAN_POINT ( 'NONE',  ( 2.449293598294706513E-15, -20.00000000000000000, -9.999999999999994671 ) ) ;
#8023 = CARTESIAN_POINT ( 'NONE',  ( 45.27934281921075410, 53.29948385550240886, -6.458785618021043895 ) ) ;
#8024 = ORIENTED_EDGE ( 'NONE', *, *, #8471, .T. ) ;
#8025 = ITEM_DEFINED_TRANSFORMATION ( 'NONE', 'NONE', #5519,  #430 ) ;
#8026 = VERTEX_POINT ( 'NONE', #12664 ) ;
#8027 = ORIENTED_EDGE ( 'NONE', *, *, #12694, .T. ) ;
#8028 = ORIENTED_EDGE ( 'NONE', *, *, #2427, .F. ) ;
#8029 = LINE ( 'NONE', #11845, #10781 ) ;
#8030 = CARTESIAN_POINT ( 'NONE',  ( 32.49999999999998579, 5.000000000000018652, -4.999999999999996447 ) ) ;
#8031 = CARTESIAN_POINT ( 'NONE',  ( 0.000000000000000000, 0.000000000000000000, -0.2800830152838844622 ) ) ;
#8032 = CARTESIAN_POINT ( 'NONE',  ( 3.806834918298644954, -3.031088913245536975, 1.750000000000000666 ) ) ;
#8033 = CARTESIAN_POINT ( 'NONE',  ( 0.000000000000000000, 0.000000000000000000, 5.000000000000000000 ) ) ;
#8034 = CARTESIAN_POINT ( 'NONE',  ( 50.02271294988511841, 60.49948385550240459, 6.000000000000000888 ) ) ;
#8035 = CARTESIAN_POINT ( 'NONE',  ( 54.13287192849671214, 54.70051614449766220, -5.649768623646139964 ) ) ;
#8036 = ADVANCED_FACE ( 'NONE', ( #153 ), #11636, .T. ) ;
#8037 = CARTESIAN_POINT ( 'NONE',  ( 45.31609314410960820, 62.30051614449766362, -6.485486291978072693 ) ) ;
#8038 = DIRECTION ( 'NONE',  ( -0.9989677110047504582, -0.04542589977017007230, 1.386346192018204258E-14 ) ) ;
#8039 = CARTESIAN_POINT ( 'NONE',  ( 49.99999999999997158, 45.00000000000001421, -6.500000000000004441 ) ) ;
#8040 = CARTESIAN_POINT ( 'NONE',  ( 49.97728705011495265, 61.50051614449765935, 7.000000000000000888 ) ) ;
#8042 = ORIENTED_EDGE ( 'NONE', *, *, #2467, .F. ) ;
#8041 = EDGE_LOOP ( 'NONE', ( #7042, #5705, #5007 ) ) ;
#8043 = CARTESIAN_POINT ( 'NONE',  ( 0.000000000000000000, 0.000000000000000000, 0.000000000000000000 ) ) ;
#8044 = EDGE_CURVE ( 'NONE', #5739, #3958, #5567, .T. ) ;
#8045 = VECTOR ( 'NONE', #4798, 1000.000000000000227 ) ;
#8046 = ORIENTED_EDGE ( 'NONE', *, *, #7525, .F. ) ;
#8047 = EDGE_CURVE ( 'NONE', #6120, #10476, #2459, .T. ) ;
#8048 = LINE ( 'NONE', #12258, #2298 ) ;
#8049 = CIRCLE ( 'NONE', #3851, 3.500000000000000000 ) ;
#8050 = DIRECTION ( 'NONE',  ( -1.000000000000000000, -0.000000000000000000, -0.000000000000000000 ) ) ;
#8051 = APPLICATION_CONTEXT ( 'automotive_design' ) ;
#8052 = EDGE_CURVE ( 'NONE', #13432, #3165, #5427, .T. ) ;
#8053 = PRODUCT_CONTEXT ( 'NONE', #3806, 'mechanical' ) ;
#8054 = CARTESIAN_POINT ( 'NONE',  ( 52.29715082351547295, 64.39948385550239607, 6.992620115222774047 ) ) ;
#8055 = CARTESIAN_POINT ( 'NONE',  ( 45.90387839640214196, 56.69948385550240744, 5.676469297603166098 ) ) ;
#8056 = VECTOR ( 'NONE', #5590, 1000.000000000000000 ) ;
#8057 = CARTESIAN_POINT ( 'NONE',  ( 10.00000000000000000, 0.000000000000000000, 9.999999999999998224 ) ) ;
#8058 = AXIS2_PLACEMENT_3D ( 'NONE', #5604, #4559, #9612 ) ;
#8059 = CARTESIAN_POINT ( 'NONE',  ( -74.99999999999997158, -7.499999999999971578, -20.00000000000000000 ) ) ;
#8060 = DIRECTION ( 'NONE',  ( 0.000000000000000000, 0.000000000000000000, 1.000000000000000000 ) ) ;
#8061 = CARTESIAN_POINT ( 'NONE',  ( 52.29715082351538769, 44.60051614449766788, -6.992620115222796251 ) ) ;
#8062 = CARTESIAN_POINT ( 'NONE',  ( 48.07319477248768180, 52.59948385550240602, 6.007379884777225953 ) ) ;
#8063 = CARTESIAN_POINT ( 'NONE',  ( -59.84999999999998721, 32.50000000000001421, -10.00000000000000178 ) ) ;
#8064 = EDGE_LOOP ( 'NONE', ( #7131, #2922, #7293, #1507 ) ) ;
#8065 = ORIENTED_EDGE ( 'NONE', *, *, #5389, .T. ) ;
#8066 = ORIENTED_EDGE ( 'NONE', *, *, #11077, .F. ) ;
#8067 = CARTESIAN_POINT ( 'NONE',  ( 4.082498951862917558, -2.020725942163694722, -3.499999999999999556 ) ) ;
#8068 = AXIS2_PLACEMENT_3D ( 'NONE', #2119, #11865, #6625 ) ;
#8069 = CARTESIAN_POINT ( 'NONE',  ( 6.207530437345012864, 4.849805425595251407, -1.599890596046337210 ) ) ;
#8070 = EDGE_CURVE ( 'NONE', #12476, #13619, #11767, .T. ) ;
#8071 = CARTESIAN_POINT ( 'NONE',  ( 62.49999999999998579, 32.50000000000001421, -9.999999999999998224 ) ) ;
#8072 = EDGE_CURVE ( 'NONE', #2996, #4555, #8794, .T. ) ;
#8073 = DIRECTION ( 'NONE',  ( 0.000000000000000000, 0.4999999999999989453, -0.8660254037844391517 ) ) ;
#8074 = PRESENTATION_STYLE_ASSIGNMENT (( #1177 ) ) ;
#8075 = LINE ( 'NONE', #1622, #5320 ) ;
#8076 = CARTESIAN_POINT ( 'NONE',  ( 44.88205777487401349, 47.80051614449764941, 3.688883143319584779 ) ) ;
#8077 = DIRECTION ( 'NONE',  ( -0.000000000000000000, -0.000000000000000000, 1.000000000000000000 ) ) ;
#8078 = CARTESIAN_POINT ( 'NONE',  ( 44.05948171654949874, 60.79948385550240886, 4.345558710429105354 ) ) ;
#8079 = CARTESIAN_POINT ( 'NONE',  ( 57.36023556966787851, 51.99948385550238328, -0.02388180880522424582 ) ) ;
#8080 = ORIENTED_EDGE ( 'NONE', *, *, #9814, .F. ) ;
#8081 = CARTESIAN_POINT ( 'NONE',  ( 55.96859303347804371, 46.19948385550238612, 4.306917132069425946 ) ) ;
#8082 = VERTEX_POINT ( 'NONE', #12925 ) ;
#8083 = ORIENTED_EDGE ( 'NONE', *, *, #7053, .F. ) ;
#8084 = DIRECTION ( 'NONE',  ( 1.000000000000000000, 0.000000000000000000, 0.000000000000000000 ) ) ;
#8085 = EDGE_LOOP ( 'NONE', ( #9425, #9641, #247, #11110 ) ) ;
#8086 = CARTESIAN_POINT ( 'NONE',  ( 0.3126073911695746443, -2.020725942163797750, -3.499999999999999556 ) ) ;
#8087 = ADVANCED_FACE ( 'NONE', ( #1307 ), #9531, .T. ) ;
#8088 = ADVANCED_FACE ( 'NONE', ( #3612 ), #2563, .F. ) ;
#8089 = CARTESIAN_POINT ( 'NONE',  ( 6.518095160331714766, -2.933089652807550074, -5.080260301817226321 ) ) ;
#8090 = CARTESIAN_POINT ( 'NONE',  ( 51.97223112728249816, 58.60051614449766788, -5.992620115222793586 ) ) ;
#8091 = AXIS2_PLACEMENT_3D ( 'NONE', #9625, #2418, #151 ) ;
#8092 = CARTESIAN_POINT ( 'NONE',  ( 4.203935335434060505, 1.640780671294165272, -3.598452447879202598 ) ) ;
#8093 = CARTESIAN_POINT ( 'NONE',  ( 42.39856655714566358, 58.89948385550241028, 2.493737253992119207 ) ) ;
#8094 = CARTESIAN_POINT ( 'NONE',  ( -30.00000000000000000, -1.040834085586084257E-14, 0.000000000000000000 ) ) ;
#8095 = CARTESIAN_POINT ( 'NONE',  ( -2.595115354961444076, -7.673029147243174641, 0.000000000000000000 ) ) ;
#8096 = CARTESIAN_POINT ( 'NONE',  ( 54.72065718078924590, 50.29948385550240886, 6.458785618021043895 ) ) ;
#8097 = ORIENTED_EDGE ( 'NONE', *, *, #12695, .T. ) ;
#8098 = VERTEX_POINT ( 'NONE', #3539 ) ;
#8099 = EDGE_LOOP ( 'NONE', ( #3481, #11092, #3604, #6867 ) ) ;
#8100 = ORIENTED_EDGE ( 'NONE', *, *, #849, .T. ) ;
#8101 = DIRECTION ( 'NONE',  ( 0.000000000000000000, 0.000000000000000000, 1.000000000000000000 ) ) ;
#8102 = VECTOR ( 'NONE', #2137, 1000.000000000000000 ) ;
#8103 = LINE ( 'NONE', #6041, #12969 ) ;
#8104 = CARTESIAN_POINT ( 'NONE',  ( 2.000000000000000000, 1.329782007511006281, 0.7677499999999984892 ) ) ;
#8105 = CARTESIAN_POINT ( 'NONE',  ( 4.000000000000000000, -2.309401076758514915, -3.433295621305383349 ) ) ;
#8106 = CARTESIAN_POINT ( 'NONE',  ( 30.00000000000000355, -40.00000000000000000, 10.00000000000000000 ) ) ;
#8107 = CARTESIAN_POINT ( 'NONE',  ( 46.45491332379572924, 65.29948385550241596, -4.840751629271157874 ) ) ;
#8108 = CARTESIAN_POINT ( 'NONE',  ( 54.09612160359792199, 51.30051614449766362, 5.676469297603124353 ) ) ;
#8109 = CARTESIAN_POINT ( 'NONE',  ( 57.61547081786810764, 56.90051614449767214, -2.450534656007114176 ) ) ;
#8110 = CARTESIAN_POINT ( 'NONE',  ( 0.000000000000000000, 0.000000000000000000, 0.000000000000000000 ) ) ;
#8111 = EDGE_CURVE ( 'NONE', #10142, #178, #1376, .T. ) ;
#8112 = CARTESIAN_POINT ( 'NONE',  ( 57.61547081786810764, 52.90051614449766504, -2.450534656007114176 ) ) ;
#8113 = B_SPLINE_CURVE_WITH_KNOTS ( 'NONE', 3,
 ( #1948, #6193, #9489, #2148, #10458, #8525, #11572, #7427, #10662, #1173, #972, #5224, #901, #12726, #6396, #10594 ),
 .UNSPECIFIED., .F., .F.,
 ( 4, 3, 3, 3, 3, 4 ),
 ( -2.669610558406242719E-06, 0.000000000000000000, 5.703179328865551904E-05, 0.0001157653700805886653, 0.0001686517580799675017, 0.0002219032271235110720 ),
 .UNSPECIFIED. ) ;
#8115 = ORIENTED_EDGE ( 'NONE', *, *, #12563, .T. ) ;
#8114 = ORIENTED_EDGE ( 'NONE', *, *, #13481, .F. ) ;
#8116 = CARTESIAN_POINT ( 'NONE',  ( -0.3198814748697807464, -4.434118497892185040, -0.3507732604232532969 ) ) ;
#8117 = ORIENTED_EDGE ( 'NONE', *, *, #8566, .F. ) ;
#8118 = ORIENTED_EDGE ( 'NONE', *, *, #662, .T. ) ;
#8119 = CARTESIAN_POINT ( 'NONE',  ( 0.1999999999999987899, 0.000000000000000000, 0.000000000000000000 ) ) ;
#8120 = DIRECTION ( 'NONE',  ( -1.000000000000000000, 0.000000000000000000, 0.000000000000000000 ) ) ;
#8121 = SHAPE_DEFINITION_REPRESENTATION ( #3124, #4503 ) ;
#8122 = CARTESIAN_POINT ( 'NONE',  ( 55.11794222512601493, 46.19948385550240744, 3.688883143319541702 ) ) ;
#8123 = CARTESIAN_POINT ( 'NONE',  ( 55.96859303347805081, 56.19948385550240744, 4.306917132069425058 ) ) ;
#8124 = LINE ( 'NONE', #12468, #13501 ) ;
#8125 = DIRECTION ( 'NONE',  ( -0.000000000000000000, -0.000000000000000000, -1.000000000000000000 ) ) ;
#8126 = CARTESIAN_POINT ( 'NONE',  ( -13.67449106481169530, -13.83491329190050578, -9.000000000000000000 ) ) ;
#8127 = CARTESIAN_POINT ( 'NONE',  ( 55.96859303347802239, 48.80051614449766362, -4.306917132069484566 ) ) ;
#8128 = CARTESIAN_POINT ( 'NONE',  ( 49.97728705011488870, 51.49948385550240459, -6.000000000000000888 ) ) ;
#8129 = DIRECTION ( 'NONE',  ( 0.000000000000000000, 0.000000000000000000, 1.000000000000000000 ) ) ;
#8130 = EDGE_CURVE ( 'NONE', #3999, #1878, #12861, .T. ) ;
#8131 = VERTEX_POINT ( 'NONE', #8866 ) ;
#8132 = EDGE_CURVE ( 'NONE', #3300, #5185, #8217, .T. ) ;
#8133 = ORIENTED_EDGE ( 'NONE', *, *, #10083, .T. ) ;
#8134 = EDGE_LOOP ( 'NONE', ( #6888, #4797, #11195, #9954 ) ) ;
#8135 = CARTESIAN_POINT ( 'NONE',  ( 4.114405500665255566, -2.025575754679718177, -3.508400121684934980 ) ) ;
#8136 = MECHANICAL_DESIGN_GEOMETRIC_PRESENTATION_REPRESENTATION (  '', ( #13629 ), #11434 ) ;
#8137 = DIRECTION ( 'NONE',  ( -1.000000000000000000, 0.000000000000000000, 0.000000000000000000 ) ) ;
#8138 = CARTESIAN_POINT ( 'NONE',  ( 6.095473853218072335, -3.806361898857768544, -3.407187799184005161 ) ) ;
#8139 = CARTESIAN_POINT ( 'NONE',  ( 43.34962307344081012, 46.89948385550240317, 2.184720259617164650 ) ) ;
#8140 = CARTESIAN_POINT ( 'NONE',  ( 53.50000000000000000, 0.000000000000000000, 0.000000000000000000 ) ) ;
#8141 = FACE_OUTER_BOUND ( 'NONE', #7702, .T. ) ;
#8142 = CARTESIAN_POINT ( 'NONE',  ( 48.02776887271745210, 65.39948385550239607, -5.992620115222778487 ) ) ;
#8143 = CARTESIAN_POINT ( 'NONE',  ( -62.49999999999997158, 20.00000000000001421, -15.00000000000000000 ) ) ;
#8144 = CARTESIAN_POINT ( 'NONE',  ( 55.96859303347804371, 60.19948385550240744, 4.306917132069425946 ) ) ;
#8145 = CARTESIAN_POINT ( 'NONE',  ( 44.03140696652192787, 51.19948385550238612, -4.306917132069425058 ) ) ;
#8146 = AXIS2_PLACEMENT_3D ( 'NONE', #7256, #1844, #1916 ) ;
#8147 = EDGE_LOOP ( 'NONE', ( #12303, #6106, #11057, #1595 ) ) ;
#8148 = EDGE_CURVE ( 'NONE', #5736, #7289, #13649, .T. ) ;
#8149 = CARTESIAN_POINT ( 'NONE',  ( 43.34962307344081012, 48.89948385550240317, 2.184720259617164650 ) ) ;
#8150 = EDGE_CURVE ( 'NONE', #9080, #11927, #11737, .T. ) ;
#8151 = EDGE_LOOP ( 'NONE', ( #3654, #9873, #3451, #896 ) ) ;
#8152 = DIRECTION ( 'NONE',  ( 1.000000000000000000, 0.000000000000000000, -0.000000000000000000 ) ) ;
#8153 = ORIENTED_EDGE ( 'NONE', *, *, #11191, .F. ) ;
#8154 = ADVANCED_FACE ( 'NONE', ( #12995 ), #10930, .T. ) ;
#8155 = CARTESIAN_POINT ( 'NONE',  ( 4.175326769692855322, 2.060699556488906126, 3.569236330973482030 ) ) ;
#8156 = CONICAL_SURFACE ( 'NONE', #2619, 5.000000000000000000, 1.047197551196600296 ) ;
#8157 = CYLINDRICAL_SURFACE ( 'NONE', #10258, 1.999999999999998224 ) ;
#8158 = CARTESIAN_POINT ( 'NONE',  ( 62.49999999999998579, 45.00000000000001421, 0.000000000000000000 ) ) ;
#8159 = VECTOR ( 'NONE', #4269, 1000.000000000000000 ) ;
#8160 = CARTESIAN_POINT ( 'NONE',  ( 55.69932041026405045, 61.10051614449766788, 1.875703265242156359 ) ) ;
#8161 = DIRECTION ( 'NONE',  ( 1.000000000000000000, 0.000000000000000000, 0.000000000000000000 ) ) ;
#8162 = CARTESIAN_POINT ( 'NONE',  ( 43.20883090819745576, 56.79948385550240175, 4.963592699179006473 ) ) ;
#8163 = CARTESIAN_POINT ( 'NONE',  ( 44.05948171654949874, 62.79948385550241596, 4.345558710429105354 ) ) ;
#8164 = DIRECTION ( 'NONE',  ( 0.000000000000000000, -1.000000000000000000, 0.000000000000000000 ) ) ;
#8165 = STYLED_ITEM ( 'NONE', ( #8965 ), #8490 ) ;
#8166 = CARTESIAN_POINT ( 'NONE',  ( 47.42335538002188144, 52.59948385550240602, 8.007379884777233059 ) ) ;
#8167 = ORIENTED_EDGE ( 'NONE', *, *, #6440, .T. ) ;
#8168 = ORIENTED_EDGE ( 'NONE', *, *, #9643, .F. ) ;
#8169 = ORIENTED_EDGE ( 'NONE', *, *, #6474, .T. ) ;
#8170 = CARTESIAN_POINT ( 'NONE',  ( 12.99038105676649835, -12.49999999999984901, 9.000000000000000000 ) ) ;
#8171 = LINE ( 'NONE', #5895, #4375 ) ;
#8172 = LINE ( 'NONE', #10171, #7789 ) ;
#8173 = CARTESIAN_POINT ( 'NONE',  ( 4.071447262713887127, -2.020725942163686284, 3.500000000000000444 ) ) ;
#8174 = CARTESIAN_POINT ( 'NONE',  ( 6.534838248920896930, -2.951765777552406878, 5.112608298763836601 ) ) ;
#8175 = CARTESIAN_POINT ( 'NONE',  ( 62.49999999999998579, 45.00000000000001421, 5.000000000000000000 ) ) ;
#8176 = AXIS2_PLACEMENT_3D ( 'NONE', #11739, #9931, #10830 ) ;
#8177 = CARTESIAN_POINT ( 'NONE',  ( 44.88205777487398507, 63.19948385550240744, -3.688883143319540814 ) ) ;
#8178 = CARTESIAN_POINT ( 'NONE',  ( 49.97728705011495265, 53.50051614449765935, 7.000000000000000888 ) ) ;
#8179 = CARTESIAN_POINT ( 'NONE',  ( 56.81924384183006538, 56.80051614449764941, -4.924951120819380357 ) ) ;
#8180 = CARTESIAN_POINT ( 'NONE',  ( 2.449293598294706513E-15, -20.00000000000000000, 15.00000000000000355 ) ) ;
#8181 = CARTESIAN_POINT ( 'NONE',  ( 45.27934281921082516, 47.70051614449766220, 6.458785618021089192 ) ) ;
#8183 = ORIENTED_EDGE ( 'NONE', *, *, #12012, .T. ) ;
#8182 = ORIENTED_EDGE ( 'NONE', *, *, #1875, .T. ) ;
#8184 = AXIS2_PLACEMENT_3D ( 'NONE', #7649, #10619, #5574 ) ;
#8185 = EDGE_LOOP ( 'NONE', ( #7005, #7554, #1155, #234 ) ) ;
#8186 = PRODUCT_DEFINITION_CONTEXT ( 'detailed design', #8051, 'design' ) ;
#8187 = ORIENTED_EDGE ( 'NONE', *, *, #4599, .F. ) ;
#8188 = ORIENTED_EDGE ( 'NONE', *, *, #10999, .T. ) ;
#8189 = CARTESIAN_POINT ( 'NONE',  ( 0.08165819712376902462, 3.720292241887087403, -3.556264818047239817 ) ) ;
#8190 = PLANE ( 'NONE',  #12832 ) ;
#8191 = PRODUCT_CONTEXT ( 'NONE', #9727, 'mechanical' ) ;
#8192 = CARTESIAN_POINT ( 'NONE',  ( 45.90387839640214196, 62.69948385550240744, 5.676469297603166098 ) ) ;
#8193 = EDGE_CURVE ( 'NONE', #11112, #10143, #10860, .T. ) ;
#8194 = CARTESIAN_POINT ( 'NONE',  ( 55.94051828345050836, 57.79948385550240175, -4.345558710429103577 ) ) ;
#8195 = CARTESIAN_POINT ( 'NONE',  ( 5.100000000000002309, 6.368163355566238354E-16, -5.200000000000001066 ) ) ;
#8196 = PRODUCT_RELATED_PRODUCT_CATEGORY ( 'part', '', ( #2235 ) ) ;
#8197 = DIRECTION ( 'NONE',  ( 1.000000000000000000, 0.000000000000000000, 0.000000000000000000 ) ) ;
#8198 = DIRECTION ( 'NONE',  ( 0.000000000000000000, 0.000000000000000000, 1.000000000000000000 ) ) ;
#8199 = CARTESIAN_POINT ( 'NONE',  ( 55.94051828345053679, 49.20051614449766930, 4.345558710429044069 ) ) ;
#8200 = CARTESIAN_POINT ( 'NONE',  ( 56.30877334542961421, 51.99948385550239749, -0.02388180880520959434 ) ) ;
#8201 = DIRECTION ( 'NONE',  ( -0.4999999999999924505, -0.8660254037844429265, 0.000000000000000000 ) ) ;
#8202 = ORIENTED_EDGE ( 'NONE', *, *, #4576, .T. ) ;
#8203 = DIRECTION ( 'NONE',  ( -0.000000000000000000, 1.000000000000000000, -0.000000000000000000 ) ) ;
#8204 = EDGE_LOOP ( 'NONE', ( #9236, #3967 ) ) ;
#8205 = ORIENTED_EDGE ( 'NONE', *, *, #3551, .F. ) ;
#8206 = DIRECTION ( 'NONE',  ( 1.000000000000000000, 0.000000000000000000, 0.000000000000000000 ) ) ;
#8207 = CARTESIAN_POINT ( 'NONE',  ( 6.212068001623052282, 5.350125758160769962, -0.7333103599825900876 ) ) ;
#8208 = DIRECTION ( 'NONE',  ( 0.000000000000000000, 0.000000000000000000, 1.000000000000000000 ) ) ;
#8209 =( LENGTH_UNIT ( ) NAMED_UNIT ( * ) SI_UNIT ( .MILLI., .METRE. ) );
#8210 = CARTESIAN_POINT ( 'NONE',  ( 54.09612160359786515, 47.69948385550240744, -5.676469297603166098 ) ) ;
#8211 = DIRECTION ( 'NONE',  ( -9.710251638871371392E-17, -5.969973981896233748E-17, -1.000000000000000000 ) ) ;
#8212 = CARTESIAN_POINT ( 'NONE',  ( 3.951447005078450925, -2.357513599190977249, -2.916666666666666519 ) ) ;
#8213 = CARTESIAN_POINT ( 'NONE',  ( 53.50833635130544508, 47.30051614449766362, 4.867452303228181343 ) ) ;
#8214 = CARTESIAN_POINT ( 'NONE',  ( 10.00000000000000000, 15.00000000000001776, -9.999999999999998224 ) ) ;
#8215 = CARTESIAN_POINT ( 'NONE',  ( 47.70284917648453415, 59.39948385550241028, -6.992620115222774047 ) ) ;
#8216 = CARTESIAN_POINT ( 'NONE',  ( 42.63976443033212860, 50.99948385550240459, 0.02388180880522514787 ) ) ;
#8217 = CIRCLE ( 'NONE', #2234, 5.000000000000000888 ) ;
#8218 = EDGE_CURVE ( 'NONE', #7877, #3166, #13135, .T. ) ;
#8219 = ORIENTED_EDGE ( 'NONE', *, *, #5497, .F. ) ;
#8220 = CARTESIAN_POINT ( 'NONE',  ( 45.86712807150323812, 47.29948385550240886, -5.649768623646098220 ) ) ;
#8221 = ORIENTED_EDGE ( 'NONE', *, *, #12263, .T. ) ;
#8222 = CARTESIAN_POINT ( 'NONE',  ( 62.49999999999998579, 45.00000000000001421, 15.00000000000000000 ) ) ;
#8223 = ORIENTED_EDGE ( 'NONE', *, *, #5560, .T. ) ;
#8224 = EDGE_CURVE ( 'NONE', #5946, #10489, #4648, .T. ) ;
#8225 = CARTESIAN_POINT ( 'NONE',  ( 4.151274195509679465, 2.039912954708742898, 3.533232880573493606 ) ) ;
#8226 = VECTOR ( 'NONE', #12960, 1000.000000000000000 ) ;
#8227 = DIRECTION ( 'NONE',  ( -0.000000000000000000, 1.000000000000000000, -0.000000000000000000 ) ) ;
#8228 = VECTOR ( 'NONE', #6202, 1000.000000000000114 ) ;
#8229 = DIRECTION ( 'NONE',  ( -0.000000000000000000, -0.000000000000000000, -1.000000000000000000 ) ) ;
#8230 = EDGE_CURVE ( 'NONE', #9042, #10003, #3548, .T. ) ;
#8231 = CARTESIAN_POINT ( 'NONE',  ( 48.02776887271750184, 63.60051614449764656, 5.992620115222795363 ) ) ;
#8232 = ADVANCED_FACE ( 'NONE', ( #11975 ), #9730, .F. ) ;
#8233 = CARTESIAN_POINT ( 'NONE',  ( 4.000000000000000000, -2.511475576507276042, -3.469253905236643565 ) ) ;
#8234 =( BOUNDED_CURVE ( )  B_SPLINE_CURVE ( 2, ( #4511, #413, #3407, #5555, #12112, #3475, #9894, #1379, #2633, #10933, #9767, #10864, #3679, #1310, #12864, #7836, #12048, #4581, #2566, #4721, #1448, #12999, #7694, #8738, #4651, #5694, #10994, #4442, #8869, #8939, #5764, #288, #1518, #480, #11063, #10791, #12928, #8797, #5625, #13138, #7902, #6859, #1585, #9835, #10030, #7629, #11833, #2356, #6593, #11903, #3542, #7766, #11979, #2425, #354, #2498, #12179, #2916, #5068, #11136, #11205, #5973, #2779, #9282, #6046, #6183, #8108, #13472, #3746, #2989, #12312, #7142, #8248, #6115, #10238, #6929, #2704, #751, #11349, #1726, #4022, #3816, #606, #1656, #545, #5900, #10175, #1936, #8178, #3882, #677, #5000, #10097, #11279, #4930, #2845, #9000, #4789, #7068, #10309, #8035, #13197, #1871, #7967, #4859, #9074, #9142, #12247, #9213, #13268, #7000, #12448, #3949, #13335, #1799, #816, #13403, #12382, #7211, #11416, #3189, #2010, #3119, #9616, #7280, #891, #5342, #73, #10515, #9548, #10651, #12652, #11492, #9351, #2140, #7479, #1027, #9477, #2074, #12518, #6323, #11684, #6258, #7419, #10582, #3324, #3050, #10449, #5276, #7352, #11625, #4293, #2, #13546, #4225, #8381, #6385, #139, #4097, #6448, #8517, #8446, #1090, #12717, #2205, #4359, #12588, #3258, #12780, #9418, #1165, #5411, #8578, #7542, #11752, #957, #2270, #10379, #5143, #8318, #5216, #11564, #13615, #4157, #6577, #12846, #12092, #11816, #7678, #7887, #399, #9817, #11886, #2479, #2339, #3525, #2407, #337, #1229 ),
 .UNSPECIFIED., .F., .F. ) 
 B_SPLINE_CURVE_WITH_KNOTS ( ( 3, 2, 2, 2, 2, 2, 2, 2, 2, 2, 2, 2, 2, 2, 2, 2, 2, 2, 2, 2, 2, 2, 2, 2, 2, 2, 2, 2, 2, 2, 2, 2, 2, 2, 2, 2, 2, 2, 2, 2, 2, 2, 2, 2, 2, 2, 2, 2, 2, 2, 2, 2, 2, 2, 2, 2, 2, 2, 2, 2, 2, 2, 2, 2, 2, 2, 2, 2, 2, 2, 2, 2, 2, 2, 2, 2, 2, 2, 2, 2, 2, 2, 2, 2, 2, 2, 2, 2, 2, 2, 2, 2, 2, 2, 2, 2, 2, 2, 2, 3 ),
 ( 0.01230184727895902198, 0.02000000000000000042, 0.02999999999999999889, 0.04000000000000000083, 0.05000000000000000278, 0.05999999999999999778, 0.07000000000000000666, 0.08000000000000000167, 0.08999999999999999667, 0.1000000000000000056, 0.1100000000000000006, 0.1199999999999999956, 0.1300000000000000044, 0.1400000000000000133, 0.1499999999999999944, 0.1600000000000000033, 0.1700000000000000122, 0.1799999999999999933, 0.1900000000000000022, 0.2000000000000000111, 0.2099999999999999922, 0.2200000000000000011, 0.2300000000000000100, 0.2399999999999999911, 0.2500000000000000000, 0.2600000000000000089, 0.2700000000000000178, 0.2800000000000000266, 0.2899999999999999800, 0.2999999999999999889, 0.3099999999999999978, 0.3200000000000000067, 0.3300000000000000155, 0.3400000000000000244, 0.3499999999999999778, 0.3599999999999999867, 0.3699999999999999956, 0.3800000000000000044, 0.3900000000000000133, 0.4000000000000000222, 0.4099999999999999756, 0.4199999999999999845, 0.4299999999999999933, 0.4400000000000000022, 0.4500000000000000111, 0.4600000000000000200, 0.4699999999999999734, 0.4799999999999999822, 0.4899999999999999911, 0.5000000000000000000, 0.5100000000000000089, 0.5200000000000000178, 0.5300000000000000266, 0.5400000000000000355, 0.5500000000000000444, 0.5600000000000000533, 0.5699999999999999512, 0.5799999999999999600, 0.5899999999999999689, 0.5999999999999999778, 0.6099999999999999867, 0.6199999999999999956, 0.6300000000000000044, 0.6400000000000000133, 0.6500000000000000222, 0.6600000000000000311, 0.6700000000000000400, 0.6800000000000000488, 0.6899999999999999467, 0.6999999999999999556, 0.7099999999999999645, 0.7199999999999999734, 0.7299999999999999822, 0.7399999999999999911, 0.7500000000000000000, 0.7600000000000000089, 0.7700000000000000178, 0.7800000000000000266, 0.7900000000000000355, 0.8000000000000000444, 0.8100000000000000533, 0.8199999999999999512, 0.8299999999999999600, 0.8399999999999999689, 0.8499999999999999778, 0.8599999999999999867, 0.8699999999999999956, 0.8800000000000000044, 0.8900000000000000133, 0.9000000000000000222, 0.9100000000000000311, 0.9200000000000000400, 0.9300000000000000488, 0.9399999999999999467, 0.9499999999999999556, 0.9599999999999999645, 0.9699999999999999734, 0.9799999999999999822, 0.9899999999999999911, 1.000000000000000000 ),
 .UNSPECIFIED. ) 
 CURVE ( )  GEOMETRIC_REPRESENTATION_ITEM ( )  RATIONAL_B_SPLINE_CURVE ( ( 0.9826544568871729002, 0.9623225587740311671, 1.000000000000000000, 0.9510565162951535312, 1.000000000000000000, 0.9510565162951535312, 1.000000000000000000, 0.9510565162951535312, 1.000000000000000000, 0.9510565162951535312, 1.000000000000000000, 0.9510565162951535312, 1.000000000000000000, 0.9510565162951535312, 1.000000000000000000, 0.9510565162951535312, 1.000000000000000000, 0.9510565162951535312, 1.000000000000000000, 0.9510565162951535312, 1.000000000000000000, 0.9510565162951535312, 1.000000000000000000, 0.9510565162951535312, 1.000000000000000000, 0.9510565162951535312, 1.000000000000000000, 0.9510565162951535312, 1.000000000000000000, 0.9510565162951535312, 1.000000000000000000, 0.9510565162951535312, 1.000000000000000000, 0.9510565162951535312, 1.000000000000000000, 0.9510565162951535312, 1.000000000000000000, 0.9510565162951535312, 1.000000000000000000, 0.9510565162951535312, 1.000000000000000000, 0.9510565162951535312, 1.000000000000000000, 0.9510565162951535312, 1.000000000000000000, 0.9510565162951535312, 1.000000000000000000, 0.9510565162951535312, 1.000000000000000000, 0.9510565162951535312, 1.000000000000000000, 0.9510565162951535312, 1.000000000000000000, 0.9510565162951535312, 1.000000000000000000, 0.9510565162951535312, 1.000000000000000000, 0.9510565162951535312, 1.000000000000000000, 0.9510565162951535312, 1.000000000000000000, 0.9510565162951535312, 1.000000000000000000, 0.9510565162951535312, 1.000000000000000000, 0.9510565162951535312, 1.000000000000000000, 0.9510565162951535312, 1.000000000000000000, 0.9510565162951535312, 1.000000000000000000, 0.9510565162951535312, 1.000000000000000000, 0.9510565162951535312, 1.000000000000000000, 0.9510565162951535312, 1.000000000000000000, 0.9510565162951535312, 1.000000000000000000, 0.9510565162951535312, 1.000000000000000000, 0.9510565162951535312, 1.000000000000000000, 0.9510565162951535312, 1.000000000000000000, 0.9510565162951535312, 1.000000000000000000, 0.9510565162951535312, 1.000000000000000000, 0.9510565162951535312, 1.000000000000000000, 0.9510565162951535312, 1.000000000000000000, 0.9510565162951535312, 1.000000000000000000, 0.9510565162951535312, 1.000000000000000000, 0.9510565162951535312, 1.000000000000000000, 0.9510565162951535312, 1.000000000000000000, 0.9510565162951535312, 1.000000000000000000, 0.9510565162951535312, 1.000000000000000000, 0.9510565162951535312, 1.000000000000000000, 0.9510565162951535312, 1.000000000000000000, 0.9510565162951535312, 1.000000000000000000, 0.9510565162951535312, 1.000000000000000000, 0.9510565162951535312, 1.000000000000000000, 0.9510565162951535312, 1.000000000000000000, 0.9510565162951535312, 1.000000000000000000, 0.9510565162951535312, 1.000000000000000000, 0.9510565162951535312, 1.000000000000000000, 0.9510565162951535312, 1.000000000000000000, 0.9510565162951535312, 1.000000000000000000, 0.9510565162951535312, 1.000000000000000000, 0.9510565162951535312, 1.000000000000000000, 0.9510565162951535312, 1.000000000000000000, 0.9510565162951535312, 1.000000000000000000, 0.9510565162951535312, 1.000000000000000000, 0.9510565162951535312, 1.000000000000000000, 0.9510565162951535312, 1.000000000000000000, 0.9510565162951535312, 1.000000000000000000, 0.9510565162951535312, 1.000000000000000000, 0.9510565162951535312, 1.000000000000000000, 0.9510565162951535312, 1.000000000000000000, 0.9510565162951535312, 1.000000000000000000, 0.9510565162951535312, 1.000000000000000000, 0.9510565162951535312, 1.000000000000000000, 0.9510565162951535312, 1.000000000000000000, 0.9510565162951535312, 1.000000000000000000, 0.9510565162951535312, 1.000000000000000000, 0.9510565162951535312, 1.000000000000000000, 0.9510565162951535312, 1.000000000000000000, 0.9510565162951535312, 1.000000000000000000, 0.9510565162951535312, 1.000000000000000000, 0.9510565162951535312, 1.000000000000000000, 0.9510565162951535312, 1.000000000000000000, 0.9510565162951535312, 1.000000000000000000, 0.9510565162951535312, 1.000000000000000000, 0.9510565162951535312, 1.000000000000000000, 0.9510565162951535312, 1.000000000000000000, 0.9510565162951535312, 1.000000000000000000, 0.9510565162951535312, 1.000000000000000000, 0.9510565162951535312, 1.000000000000000000, 0.9510565162951535312, 1.000000000000000000, 0.9510565162951535312, 1.000000000000000000, 0.9510565162951535312, 1.000000000000000000, 0.9510565162951535312, 1.000000000000000000, 0.9510565162951535312, 1.000000000000000000, 0.9510565162951535312, 1.000000000000000000 ) ) 
 REPRESENTATION_ITEM ( '' )  );
#8235 = CARTESIAN_POINT ( 'NONE',  ( 45.31609314410967926, 60.69948385550240033, 6.485486291978119766 ) ) ;
#8236 = CARTESIAN_POINT ( 'NONE',  ( -62.49999999999997158, 40.00000000000001421, 0.000000000000000000 ) ) ;
#8237 = CARTESIAN_POINT ( 'NONE',  ( 56.81924384183011512, 50.19948385550241454, 4.924951120819313743 ) ) ;
#8238 = VERTEX_POINT ( 'NONE', #2495 ) ;
#8239 = ORIENTED_EDGE ( 'NONE', *, *, #2738, .T. ) ;
#8240 = CONICAL_SURFACE ( 'NONE', #5812, 5.000000000000000000, 1.047197551196600296 ) ;
#8241 = ORIENTED_EDGE ( 'NONE', *, *, #13451, .F. ) ;
#8242 = DIRECTION ( 'NONE',  ( 0.000000000000000000, 0.000000000000000000, -1.000000000000000000 ) ) ;
#8243 = FILL_AREA_STYLE ('',( #5063 ) ) ;
#8244 = CARTESIAN_POINT ( 'NONE',  ( -75.00000000000001421, -5.000000000000025757, 6.123233995736766282E-16 ) ) ;
#8245 = CARTESIAN_POINT ( 'NONE',  ( 4.211140560182196957, 2.431303136016536470, -3.745885042887433514 ) ) ;
#8246 = CARTESIAN_POINT ( 'NONE',  ( 0.000000000000000000, 0.8865213383406680414, -1.535500000000000975 ) ) ;
#8247 = CARTESIAN_POINT ( 'NONE',  ( 46.45491332379572924, 61.29948385550240886, -4.840751629271157874 ) ) ;
#8248 = CARTESIAN_POINT ( 'NONE',  ( 43.33558569842706021, 51.90051614449765793, 2.141517661632167169 ) ) ;
#8249 = CARTESIAN_POINT ( 'NONE',  ( 47.37792948025170858, 59.60051614449765367, 7.992620115222797139 ) ) ;
#8250 = CIRCLE ( 'NONE', #10667, 1.999999999999998224 ) ;
#8251 = DIRECTION ( 'NONE',  ( 1.000000000000000000, 0.000000000000000000, 0.000000000000000000 ) ) ;
#8252 = CARTESIAN_POINT ( 'NONE',  ( 41.58830220609386430, 48.00051614449766646, -0.02388180880514929535 ) ) ;
#8254 = EDGE_LOOP ( 'NONE', ( #951, #11605, #4763, #10408 ) ) ;
#8253 = ORIENTED_EDGE ( 'NONE', *, *, #13072, .F. ) ;
#8255 = ADVANCED_FACE ( 'NONE', ( #10788 ), #2889, .T. ) ;
#8256 = VERTEX_POINT ( 'NONE', #4438 ) ;
#8257 = ORIENTED_EDGE ( 'NONE', *, *, #8680, .T. ) ;
#8258 = LINE ( 'NONE', #12530, #11097 ) ;
#8259 = DIRECTION ( 'NONE',  ( -0.000000000000000000, -0.000000000000000000, -1.000000000000000000 ) ) ;
#8260 = CARTESIAN_POINT ( 'NONE',  ( 2.354826896168714434, -6.962563485461402024, 0.000000000000000000 ) ) ;
#8261 = APPLICATION_PROTOCOL_DEFINITION ( 'draft international standard', 'automotive_design', 1998, #10163 ) ;
#8262 = CARTESIAN_POINT ( 'NONE',  ( 56.65037692655918988, 61.89948385550241028, -2.184720259617163762 ) ) ;
#8263 = CARTESIAN_POINT ( 'NONE',  ( 49.97728705011488159, 57.49948385550241170, -7.000000000000000888 ) ) ;
#8264 = B_SPLINE_CURVE_WITH_KNOTS ( 'NONE', 3,
 ( #773, #12331, #2799, #3695, #13358, #11297 ),
 .UNSPECIFIED., .F., .F.,
 ( 4, 2, 4 ),
 ( 0.000000000000000000, 0.001488912493401906576, 0.002977824986803813152 ),
 .UNSPECIFIED. ) ;
#8265 = CARTESIAN_POINT ( 'NONE',  ( 42.63976443033212860, 62.00051614449764514, -0.02388180880514948964 ) ) ;
#8266 = CARTESIAN_POINT ( 'NONE',  ( -74.99999999999997158, 20.00000000000001421, 15.00000000000000000 ) ) ;
#8267 = DIRECTION ( 'NONE',  ( -0.000000000000000000, -0.000000000000000000, 1.000000000000000000 ) ) ;
#8268 = DIRECTION ( 'NONE',  ( 0.000000000000000000, 0.000000000000000000, 1.000000000000000000 ) ) ;
#8269 = CARTESIAN_POINT ( 'NONE',  ( 49.97728705011495265, 49.50051614449765935, 7.000000000000000888 ) ) ;
#8270 = CARTESIAN_POINT ( 'NONE',  ( 48.02776887271745210, 49.39948385550241028, -5.992620115222778487 ) ) ;
#8271 = CARTESIAN_POINT ( 'NONE',  ( 7.500000000000003553, -20.00000000000000000, -20.00000000000000000 ) ) ;
#8272 = CIRCLE ( 'NONE', #3179, 4.799999999999999822 ) ;
#8273 = ORIENTED_EDGE ( 'NONE', *, *, #4265, .T. ) ;
#8274 = DIRECTION ( 'NONE',  ( -0.000000000000000000, -0.000000000000000000, 1.000000000000000000 ) ) ;
#8275 = ORIENTED_EDGE ( 'NONE', *, *, #6140, .F. ) ;
#8276 = AXIS2_PLACEMENT_3D ( 'NONE', #12334, #4742, #8958 ) ;
#8277 = ORIENTED_EDGE ( 'NONE', *, *, #9059, .F. ) ;
#8278 = DIRECTION ( 'NONE',  ( -0.8660254037844412611, 0.4999999999999956146, 0.000000000000000000 ) ) ;
#8279 = CARTESIAN_POINT ( 'NONE',  ( 75.00000000000000000, 40.00000000000000000, 10.00000000000000000 ) ) ;
#8280 = CARTESIAN_POINT ( 'NONE',  ( 6.403457969954084561, -2.888443235695444145, 5.002930439003169028 ) ) ;
#8281 = SURFACE_STYLE_USAGE ( .BOTH. , #1904 ) ;
#8282 = CARTESIAN_POINT ( 'NONE',  ( -6.000000000000012434, -7.009618943233427935, -9.000000000000000000 ) ) ;
#8283 = AXIS2_PLACEMENT_3D ( 'NONE', #5015, #5984, #1667 ) ;
#8284 = CARTESIAN_POINT ( 'NONE',  ( 6.165086708099646984, -33.67449106481162602, -9.000000000000000000 ) ) ;
#8285 = CARTESIAN_POINT ( 'NONE',  ( 55.08986747509849380, 45.20051614449766220, 3.727524721679155384 ) ) ;
#8286 = DIRECTION ( 'NONE',  ( 0.000000000000000000, 1.000000000000000000, 0.000000000000000000 ) ) ;
#8287 = AXIS2_PLACEMENT_3D ( 'NONE', #3710, #1694, #717 ) ;
#8288 = CARTESIAN_POINT ( 'NONE',  ( 52.29715082351547295, 64.39948385550239607, 6.992620115222774047 ) ) ;
#8289 = CARTESIAN_POINT ( 'NONE',  ( 50.02271294988512551, 56.49948385550240459, 7.000000000000000888 ) ) ;
#8290 = ORIENTED_EDGE ( 'NONE', *, *, #3246, .F. ) ;
#8291 = CARTESIAN_POINT ( 'NONE',  ( 50.02271294988512551, 50.49948385550240459, 7.000000000000000888 ) ) ;
#8292 = AXIS2_PLACEMENT_3D ( 'NONE', #7883, #6837, #10149 ) ;
#8293 = ORIENTED_EDGE ( 'NONE', *, *, #5011, .T. ) ;
#8294 = CARTESIAN_POINT ( 'NONE',  ( 0.000000000000000000, 0.000000000000000000, 0.000000000000000000 ) ) ;
#8295 = VERTEX_POINT ( 'NONE', #11060 ) ;
#8296 = EDGE_CURVE ( 'NONE', #4695, #13432, #142, .T. ) ;
#8297 = CARTESIAN_POINT ( 'NONE',  ( -4.000000000000000000, -2.309401076758512694, -3.433295621305382461 ) ) ;
#8298 = DIRECTION ( 'NONE',  ( -0.000000000000000000, -0.000000000000000000, -1.000000000000000000 ) ) ;
#8299 = CARTESIAN_POINT ( 'NONE',  ( 45.86712807150323812, 47.29948385550240886, -5.649768623646098220 ) ) ;
#8300 = CARTESIAN_POINT ( 'NONE',  ( 47.70284917648459100, 47.60051614449763946, 6.992620115222796251 ) ) ;
#8301 = CARTESIAN_POINT ( 'NONE',  ( -4.000000000000000000, 2.309401076758498483, -0.4999999999999927280 ) ) ;
#8302 = CARTESIAN_POINT ( 'NONE',  ( 42.38452918213188525, 61.09948385550241312, -2.450534656007040013 ) ) ;
#8303 = CARTESIAN_POINT ( 'NONE',  ( 0.1397371499203167444, 1.362866705341264195, 3.499999999999999556 ) ) ;
#8304 = FACE_OUTER_BOUND ( 'NONE', #4273, .T. ) ;
#8305 = EDGE_CURVE ( 'NONE', #725, #9956, #13241, .T. ) ;
#8306 = CARTESIAN_POINT ( 'NONE',  ( 43.20883090819745576, 52.79948385550240175, 4.963592699179006473 ) ) ;
#8307 = EDGE_CURVE ( 'NONE', #7974, #1019, #4656, .T. ) ;
#8308 = EDGE_LOOP ( 'NONE', ( #12632, #4922, #2824 ) ) ;
#8309 = ORIENTED_EDGE ( 'NONE', *, *, #134, .T. ) ;
#8310 = ADVANCED_FACE ( 'NONE', ( #13195 ), #12379, .T. ) ;
#8311 = ORIENTED_EDGE ( 'NONE', *, *, #6959, .F. ) ;
#8312 = DIRECTION ( 'NONE',  ( 1.000000000000000000, 0.000000000000000000, 0.000000000000000000 ) ) ;
#8313 = CARTESIAN_POINT ( 'NONE',  ( 20.00000000000000000, -20.00000000000000000, -23.00000000000000000 ) ) ;
#8314 = CARTESIAN_POINT ( 'NONE',  ( 6.507056315241511513, -2.833450876375909644, 5.092319121366346124 ) ) ;
#8315 =( BOUNDED_SURFACE ( )  B_SPLINE_SURFACE ( 3, 2, ( 
 ( #7615, #7544, #4228 ),
 ( #3260, #8651, #1094 ),
 ( #2273, #6519, #7681 ),
 ( #9753, #11755, #274 ),
 ( #11627, #5278, #75 ),
 ( #6652, #4495, #2207 ) ),
 .UNSPECIFIED., .F., .F., .F. ) 
 B_SPLINE_SURFACE_WITH_KNOTS ( ( 4, 2, 4 ),
 ( 3, 3 ),
 ( 0.01651999345535505245, 0.01858032176739834312, 0.02064065007944163727 ),
 ( 0.000000000000000000, 1.000000000000000000 ),
 .UNSPECIFIED. ) 
 GEOMETRIC_REPRESENTATION_ITEM ( )  RATIONAL_B_SPLINE_SURFACE ( (
 ( 1.000000000000000000, 0.8047781103519393575, 1.000000000000000000),
 ( 1.000000000000000000, 0.8123785825604844524, 1.000000000000000000),
 ( 1.000000000000000000, 0.8190671539787625077, 1.000000000000000000),
 ( 1.000000000000000000, 0.8192352254835536529, 1.000000000000000000),
 ( 1.000000000000000000, 0.8126129677211098024, 1.000000000000000000),
 ( 1.000000000000000000, 0.8047712537969730073, 1.000000000000000000) ) ) 
 REPRESENTATION_ITEM ( '' )  SURFACE ( )  );
#8316 = DIRECTION ( 'NONE',  ( 0.000000000000000000, 0.000000000000000000, 1.000000000000000000 ) ) ;
#8317 = CARTESIAN_POINT ( 'NONE',  ( 43.69122665457040000, 48.00051614449766646, -0.02388180880515696977 ) ) ;
#8318 = CARTESIAN_POINT ( 'NONE',  ( 52.29715082351539479, 62.60051614449766078, -6.992620115222796251 ) ) ;
#8319 = CARTESIAN_POINT ( 'NONE',  ( 47.42335538002180328, 56.40051614449765793, -8.007379884777206414 ) ) ;
#8320 = LINE ( 'NONE', #9215, #9984 ) ;
#8321 = CARTESIAN_POINT ( 'NONE',  ( 56.79116909180259398, 47.20051614449766220, 4.963592699178938972 ) ) ;
#8322 = AXIS2_PLACEMENT_3D ( 'NONE', #8338, #7305, #10466 ) ;
#8324 = VERTEX_POINT ( 'NONE', #748 ) ;
#8323 = ORIENTED_EDGE ( 'NONE', *, *, #5470, .T. ) ;
#8325 = CIRCLE ( 'NONE', #11839, 12.50000000000000000 ) ;
#8326 = ORIENTED_EDGE ( 'NONE', *, *, #7884, .F. ) ;
#8327 = UNCERTAINTY_MEASURE_WITH_UNIT (LENGTH_MEASURE( 1.000000000000000082E-05 ), #1931, 'distance_accuracy_value', 'NONE');
#8328 = ORIENTED_EDGE ( 'NONE', *, *, #9081, .T. ) ;
#8329 = FACE_BOUND ( 'NONE', #740, .T. ) ;
#8330 = DIRECTION ( 'NONE',  ( 0.000000000000000000, 1.000000000000000000, -1.345283343056720273E-15 ) ) ;
#8331 = CARTESIAN_POINT ( 'NONE',  ( 15.00000000000000355, -19.99999999999984368, 9.000000000000000000 ) ) ;
#8332 = CARTESIAN_POINT ( 'NONE',  ( 0.1996310553826630974, 1.947030205581109730, -5.000000000000000888 ) ) ;
#8333 = SHAPE_DEFINITION_REPRESENTATION ( #4125, #3897 ) ;
#8334 = CARTESIAN_POINT ( 'NONE',  ( 44.05948171654949874, 60.79948385550240886, 4.345558710429105354 ) ) ;
#8335 = CARTESIAN_POINT ( 'NONE',  ( 52.29715082351547295, 64.39948385550239607, 6.992620115222774047 ) ) ;
#8336 = CARTESIAN_POINT ( 'NONE',  ( 47.74827507625469281, 58.40051614449766504, -7.007379884777203749 ) ) ;
#8337 = DIRECTION ( 'NONE',  ( -0.000000000000000000, -0.000000000000000000, 1.000000000000000000 ) ) ;
#8338 = CARTESIAN_POINT ( 'NONE',  ( -5.384454397937118664, 6.594054843588581554E-16, -4.484454397937119197 ) ) ;
#8339 = CARTESIAN_POINT ( 'NONE',  ( 20.00000000000000000, -20.00000000000000000, -20.00000000000000000 ) ) ;
#8340 = CARTESIAN_POINT ( 'NONE',  ( 45.90387839640208512, 48.30051614449765651, -5.676469297603124353 ) ) ;
#8341 = CARTESIAN_POINT ( 'NONE',  ( 44.88205777487398507, 59.19948385550240744, -3.688883143319540814 ) ) ;
#8342 = DIRECTION ( 'NONE',  ( -0.000000000000000000, 0.000000000000000000, -1.000000000000000000 ) ) ;
#8343 = ORIENTED_EDGE ( 'NONE', *, *, #6133, .T. ) ;
#8344 = ADVANCED_FACE ( 'NONE', ( #1868 ), #813, .F. ) ;
#8345 = CARTESIAN_POINT ( 'NONE',  ( 5.000000000000003553, -20.00000000000000000, 9.000000000000000000 ) ) ;
#8346 = VERTEX_POINT ( 'NONE', #13265 ) ;
#8347 = EDGE_LOOP ( 'NONE', ( #5372, #6475, #6789, #489, #12527, #8187, #10783, #1737 ) ) ;
#8348 = CARTESIAN_POINT ( 'NONE',  ( 1.567478505476134606E-15, 4.618802153517012066, -3.433295621305382905 ) ) ;
#8349 = CARTESIAN_POINT ( 'NONE',  ( 6.506891779418572774, 5.826362946429627598, 0.09155664655281574305 ) ) ;
#8350 = CARTESIAN_POINT ( 'NONE',  ( -4.000000000000000000, -1.560351142792950618, -0.2242961665059814425 ) ) ;
#8351 = FILL_AREA_STYLE_COLOUR ( '', #2629 ) ;
#8352 = CARTESIAN_POINT ( 'NONE',  ( 0.1481481481481481122, -4.797713218419819903, 0.000000000000000000 ) ) ;
#8353 = CARTESIAN_POINT ( 'NONE',  ( 53.54508667620424234, 48.70051614449766930, -4.840751629271188961 ) ) ;
#8354 = DIRECTION ( 'NONE',  ( 1.000000000000000000, 0.000000000000000000, 0.000000000000000000 ) ) ;
#8355 = CARTESIAN_POINT ( 'NONE',  ( 47.70284917648453415, 63.39948385550240317, -6.992620115222774047 ) ) ;
#8356 = CARTESIAN_POINT ( 'NONE',  ( 56.65037692655918988, 55.89948385550240317, -2.184720259617163762 ) ) ;
#8357 = ORIENTED_EDGE ( 'NONE', *, *, #1116, .F. ) ;
#8358 = AXIS2_PLACEMENT_3D ( 'NONE', #2754, #7943, #4557 ) ;
#8359 = ORIENTED_EDGE ( 'NONE', *, *, #9581, .F. ) ;
#8360 = CARTESIAN_POINT ( 'NONE',  ( 4.180345472528542494, 2.086001522971430600, 3.570468649087212398 ) ) ;
#8361 = CARTESIAN_POINT ( 'NONE',  ( 4.071447262713887127, 2.020725942163688504, 3.500000000000000000 ) ) ;
#8362 = CARTESIAN_POINT ( 'NONE',  ( -0.5000000000000000000, -6.429618962271402616, 0.000000000000000000 ) ) ;
#8363 = LINE ( 'NONE', #5051, #3773 ) ;
#8364 = CARTESIAN_POINT ( 'NONE',  ( 44.03140696652198471, 45.80051614449764230, 4.306917132069485454 ) ) ;
#8365 = CIRCLE ( 'NONE', #2838, 0.7500000000000000000 ) ;
#8366 = EDGE_CURVE ( 'NONE', #2486, #568, #8997, .T. ) ;
#8367 = CARTESIAN_POINT ( 'NONE',  ( 5.000000000000003553, -20.00000000000000000, 9.999999999999998224 ) ) ;
#8368 = CARTESIAN_POINT ( 'NONE',  ( 57.36023556966787851, 45.99948385550238328, -0.02388180880522424582 ) ) ;
#8369 = CARTESIAN_POINT ( 'NONE',  ( 4.630153689607048761, 0.000000000000000000, -5.371010071662833063 ) ) ;
#8370 = ADVANCED_FACE ( 'NONE', ( #2912, #11346 ), #6112, .T. ) ;
#8371 = CARTESIAN_POINT ( 'NONE',  ( 45.27934281921075410, 55.29948385550240175, -6.458785618021043895 ) ) ;
#8372 = VERTEX_POINT ( 'NONE', #12176 ) ;
#8373 = VERTEX_POINT ( 'NONE', #4997 ) ;
#8374 = AXIS2_PLACEMENT_3D ( 'NONE', #3420, #9135, #6740 ) ;
#8375 = DIRECTION ( 'NONE',  ( 1.000000000000000000, 3.469446951953615175E-16, 0.000000000000000000 ) ) ;
#8376 = PRESENTATION_LAYER_ASSIGNMENT (  '', '', ( #397 ) ) ;
#8377 = DIRECTION ( 'NONE',  ( 0.000000000000000000, -1.224646799147353700E-16, 1.000000000000000000 ) ) ;
#8378 = CARTESIAN_POINT ( 'NONE',  ( 6.323279575526007612, -3.325091652217148308, 4.240772318536393470 ) ) ;
#8379 = CARTESIAN_POINT ( 'NONE',  ( 0.6810597143197052450, 4.461075778259290914, -3.598441714920602053 ) ) ;
#8380 = CARTESIAN_POINT ( 'NONE',  ( 43.69122665457040000, 50.00051614449765935, -0.02388180880515696977 ) ) ;
#8381 = CARTESIAN_POINT ( 'NONE',  ( 44.05948171654945611, 60.20051614449765509, -4.345558710429044069 ) ) ;
#8382 = CARTESIAN_POINT ( 'NONE',  ( 57.60143344285435774, 63.10051614449766078, 2.493737253992045044 ) ) ;
#8383 = AXIS2_PLACEMENT_3D ( 'NONE', #12647, #8242, #952 ) ;
#8384 = CARTESIAN_POINT ( 'NONE',  ( 4.000000000000000000, 0.3987449864460005378, -0.01220643443059817035 ) ) ;
#8385 = CARTESIAN_POINT ( 'NONE',  ( 54.72065718078918906, 58.70051614449765509, -6.458785618021089192 ) ) ;
#8387 = EDGE_CURVE ( 'NONE', #6599, #1223, #7750, .T. ) ;
#8386 = ORIENTED_EDGE ( 'NONE', *, *, #2210, .F. ) ;
#8388 = ORIENTED_EDGE ( 'NONE', *, *, #6621, .T. ) ;
#8389 = ORIENTED_EDGE ( 'NONE', *, *, #11991, .T. ) ;
#8390 = AXIS2_PLACEMENT_3D ( 'NONE', #3224, #1125, #6483 ) ;
#8391 = DIRECTION ( 'NONE',  ( -1.000000000000000000, 0.000000000000000000, 0.000000000000000000 ) ) ;
#8393 = AXIS2_PLACEMENT_3D ( 'NONE', #4563, #8782, #6714 ) ;
#8392 = CARTESIAN_POINT ( 'NONE',  ( 13.61000000000001009, 2.449293598294708386E-16, -2.000000000000001332 ) ) ;
#8394 = CARTESIAN_POINT ( 'NONE',  ( 30.00000000000000355, 40.00000000000000000, 0.000000000000000000 ) ) ;
#8395 = CARTESIAN_POINT ( 'NONE',  ( 0.000000000000000000, 0.000000000000000000, -5.000000000000000000 ) ) ;
#8396 = CARTESIAN_POINT ( 'NONE',  ( 44.91013252490152752, 48.79948385550240175, 3.727524721679198461 ) ) ;
#8397 = CIRCLE ( 'NONE', #11914, 12.50000000000000000 ) ;
#8398 = CARTESIAN_POINT ( 'NONE',  ( 42.63976443033212149, 64.99948385550240459, 0.02388180880522514787 ) ) ;
#8399 = EDGE_CURVE ( 'NONE', #12971, #8775, #5331, .T. ) ;
#8400 = CARTESIAN_POINT ( 'NONE',  ( 49.97728705011495265, 63.50051614449765935, 7.000000000000000888 ) ) ;
#8401 = EDGE_CURVE ( 'NONE', #6266, #3891, #9514, .T. ) ;
#8402 = CARTESIAN_POINT ( 'NONE',  ( -65.14999999999996305, 32.50000000000001421, 15.00000000000000000 ) ) ;
#8403 = DIRECTION ( 'NONE',  ( 0.000000000000000000, -0.000000000000000000, 1.000000000000000000 ) ) ;
#8404 = CARTESIAN_POINT ( 'NONE',  ( 4.055492966679587141, 3.795017426214561063, -0.5629142681441071661 ) ) ;
#8405 = CARTESIAN_POINT ( 'NONE',  ( 56.66441430157294690, 52.90051614449765793, -2.141517661632166281 ) ) ;
#8406 = CARTESIAN_POINT ( 'NONE',  ( 55.11794222512601493, 56.19948385550240744, 3.688883143319541702 ) ) ;
#8407 = VECTOR ( 'NONE', #8969, 1000.000000000000000 ) ;
#8408 = DIRECTION ( 'NONE',  ( 0.000000000000000000, 0.000000000000000000, 1.000000000000000000 ) ) ;
#8409 = ADVANCED_FACE ( 'NONE', ( #2628 ), #2701, .T. ) ;
#8410 = ORIENTED_EDGE ( 'NONE', *, *, #3251, .F. ) ;
#8411 = CARTESIAN_POINT ( 'NONE',  ( -74.99999999999997158, 20.00000000000001421, -15.00000000000000000 ) ) ;
#8412 = ORIENTED_EDGE ( 'NONE', *, *, #13535, .F. ) ;
#8413 = CARTESIAN_POINT ( 'NONE',  ( 6.518095160331712989, 2.933089652807542524, 5.080260301817225432 ) ) ;
#8414 = CARTESIAN_POINT ( 'NONE',  ( -74.99999999999997158, -39.99999999999998579, -20.00000000000000000 ) ) ;
#8415 = CARTESIAN_POINT ( 'NONE',  ( 4.175075985190094485, 2.060370777630093464, -3.568666869285578080 ) ) ;
#8416 =( GEOMETRIC_REPRESENTATION_CONTEXT ( 3 ) GLOBAL_UNCERTAINTY_ASSIGNED_CONTEXT ( ( #3435 ) ) GLOBAL_UNIT_ASSIGNED_CONTEXT ( ( #886, #2910, #7062 ) ) REPRESENTATION_CONTEXT ( 'NONE', 'WORKASPACE' ) );
#8417 = CARTESIAN_POINT ( 'NONE',  ( 47.70284917648453415, 53.39948385550238186, -6.992620115222774047 ) ) ;
#8418 = CONICAL_SURFACE ( 'NONE', #4215, 5.560781378645573980, 1.221730476396046816 ) ;
#8419 = EDGE_CURVE ( 'NONE', #9288, #4365, #13157, .T. ) ;
#8420 = DIRECTION ( 'NONE',  ( -1.000000000000000000, 0.000000000000000000, 0.000000000000000000 ) ) ;
#8421 = CARTESIAN_POINT ( 'NONE',  ( 44.91013252490150620, 54.20051614449766220, -3.727524721679154940 ) ) ;
#8422 = CARTESIAN_POINT ( 'NONE',  ( -4.197393957002303999, -7.773935952363655451E-14, -3.503767560748929810 ) ) ;
#8423 = CARTESIAN_POINT ( 'NONE',  ( 43.34962307344081012, 62.89948385550241028, 2.184720259617164650 ) ) ;
#8424 = CARTESIAN_POINT ( 'NONE',  ( 43.33558569842703179, 63.09948385550240602, -2.141517661632099223 ) ) ;
#8425 = CARTESIAN_POINT ( 'NONE',  ( 44.03140696652192787, 59.19948385550238612, -4.306917132069425058 ) ) ;
#8426 = ORIENTED_EDGE ( 'NONE', *, *, #1697, .F. ) ;
#8427 = ORIENTED_EDGE ( 'NONE', *, *, #13444, .F. ) ;
#8428 = CARTESIAN_POINT ( 'NONE',  ( 4.175572532730932096, 4.122058607836116551, 1.170198429493232648E-15 ) ) ;
#8429 = DIRECTION ( 'NONE',  ( 0.000000000000000000, 0.000000000000000000, -1.000000000000000000 ) ) ;
#8430 = CARTESIAN_POINT ( 'NONE',  ( 4.180231891692622881, -4.134807952925578789, -0.02076457676760693274 ) ) ;
#8431 = DIRECTION ( 'NONE',  ( 1.000000000000000000, 0.000000000000000000, 0.000000000000000000 ) ) ;
#8432 = DIRECTION ( 'NONE',  ( 0.000000000000000000, 1.000000000000000000, 0.000000000000000000 ) ) ;
#8433 = CARTESIAN_POINT ( 'NONE',  ( 44.05948171654945611, 50.20051614449764088, -4.345558710429044069 ) ) ;
#8434 = PRODUCT_DEFINITION_SHAPE ( 'NONE', 'NONE',  #13672 ) ;
#8435 = CARTESIAN_POINT ( 'NONE',  ( 8.759913291900563337, -32.17636723815374467, 0.000000000000000000 ) ) ;
#8436 = CARTESIAN_POINT ( 'NONE',  ( 52.25172492374522903, 47.59948385550239891, -7.007379884777225953 ) ) ;
#8437 = CARTESIAN_POINT ( 'NONE',  ( 56.79116909180255135, 55.79948385550239465, -4.963592699179005585 ) ) ;
#8438 = ORIENTED_EDGE ( 'NONE', *, *, #4620, .F. ) ;
#8439 = ORIENTED_EDGE ( 'NONE', *, *, #7884, .T. ) ;
#8440 = CIRCLE ( 'NONE', #3351, 4.000000000000003553 ) ;
#8441 = CARTESIAN_POINT ( 'NONE',  ( 75.00000000000001421, 2.602085213965211904E-14, 0.000000000000000000 ) ) ;
#8442 = CARTESIAN_POINT ( 'NONE',  ( 0.000000000000000000, 0.000000000000000000, -9.000000000000001776 ) ) ;
#8443 = DIRECTION ( 'NONE',  ( -1.000000000000000000, 0.000000000000000000, 0.000000000000000000 ) ) ;
#8444 = DIRECTION ( 'NONE',  ( -1.000000000000000000, -0.000000000000000000, -0.000000000000000000 ) ) ;
#8445 = CARTESIAN_POINT ( 'NONE',  ( 55.69932041026405045, 49.10051614449766788, 1.875703265242156359 ) ) ;
#8446 = CARTESIAN_POINT ( 'NONE',  ( 55.96859303347802239, 60.80051614449765651, -4.306917132069484566 ) ) ;
#8447 = CARTESIAN_POINT ( 'NONE',  ( 41.58830220609386430, 48.99948385550241170, 0.02388180880523263147 ) ) ;
#8448 = CONICAL_SURFACE ( 'NONE', #5798, 2.500000000000000888, 0.9599310885968785900 ) ;
#8449 = CARTESIAN_POINT ( 'NONE',  ( 3.734041964264196878, -16.98388816369253362, -9.999999999999994671 ) ) ;
#8450 = CARTESIAN_POINT ( 'NONE',  ( 41.58830220609386430, 58.00051614449765935, -0.02388180880514929535 ) ) ;
#8451 = CIRCLE ( 'NONE', #9778, 1.500000000000001110 ) ;
#8452 = EDGE_LOOP ( 'NONE', ( #7638, #6411, #538, #1473 ) ) ;
#8453 = ORIENTED_EDGE ( 'NONE', *, *, #3454, .T. ) ;
#8454 = ORIENTED_EDGE ( 'NONE', *, *, #5599, .T. ) ;
#8455 = FACE_OUTER_BOUND ( 'NONE', #11248, .T. ) ;
#8456 = CARTESIAN_POINT ( 'NONE',  ( 2.000000000000000000, -0.8865213383406694847, 1.535500000000001419 ) ) ;
#8457 = EDGE_CURVE ( 'NONE', #5420, #9576, #5538, .T. ) ;
#8458 = FACE_BOUND ( 'NONE', #4397, .T. ) ;
#8459 = FACE_BOUND ( 'NONE', #7522, .T. ) ;
#8460 = VECTOR ( 'NONE', #5128, 1000.000000000000000 ) ;
#8461 = CARTESIAN_POINT ( 'NONE',  ( 44.28664221472220675, 49.09948385550241312, -1.832500667257165317 ) ) ;
#8462 = CARTESIAN_POINT ( 'NONE',  ( 56.66441430157296821, 64.09948385550239891, 2.141517661632100111 ) ) ;
#8463 = CARTESIAN_POINT ( 'NONE',  ( 44.03140696652198471, 63.80051614449765651, 4.306917132069485454 ) ) ;
#8464 = CARTESIAN_POINT ( 'NONE',  ( 5.000000000000003553, -20.00000000000000000, 15.00000000000000355 ) ) ;
#8465 = CARTESIAN_POINT ( 'NONE',  ( 18.00000000000000355, -20.00000000000000000, -12.00000000000000000 ) ) ;
#8466 = CARTESIAN_POINT ( 'NONE',  ( 52.80949999999998568, 0.000000000000000000, 0.000000000000000000 ) ) ;
#8467 = CLOSED_SHELL ( 'NONE', ( #1438, #13446, #5777, #8087, #12924, #8154, #9549, #5215, #11704, #1093, #13107, #6038, #10099, #6293, #2803, #6273, #8310, #2451, #9522, #5034, #11431, #654, #4127, #10081, #9238, #2964, #6784 ) ) ;
#8468 = CARTESIAN_POINT ( 'NONE',  ( 56.65037692655921120, 59.10051614449766078, 2.184720259617097593 ) ) ;
#8469 = CARTESIAN_POINT ( 'NONE',  ( 55.71335778527780747, 60.09948385550240602, 1.832500667257165983 ) ) ;
#8470 = DIRECTION ( 'NONE',  ( 0.000000000000000000, 0.000000000000000000, -1.000000000000000000 ) ) ;
#8471 = EDGE_CURVE ( 'NONE', #2658, #13327, #10388, .T. ) ;
#8472 = VERTEX_POINT ( 'NONE', #3946 ) ;
#8473 = EDGE_CURVE ( 'NONE', #10472, #3498, #9070, .T. ) ;
#8474 = DIRECTION ( 'NONE',  ( -0.000000000000000000, -0.000000000000000000, 1.000000000000000000 ) ) ;
#8475 = EDGE_CURVE ( 'NONE', #3147, #347, #5106, .T. ) ;
#8476 = EDGE_LOOP ( 'NONE', ( #8182, #11497, #10147, #13503 ) ) ;
#8477 = DIRECTION ( 'NONE',  ( -1.000000000000000000, 0.000000000000000000, 0.000000000000000000 ) ) ;
#8478 = ADVANCED_FACE ( 'NONE', ( #6320 ), #2477, .F. ) ;
#8479 = DIRECTION ( 'NONE',  ( 0.000000000000000000, 0.000000000000000000, -1.000000000000000000 ) ) ;
#8480 = CARTESIAN_POINT ( 'NONE',  ( 4.151274195509685683, 2.039912954708744230, -3.533232880573500267 ) ) ;
#8481 = PRESENTATION_STYLE_ASSIGNMENT (( #2171 ) ) ;
#8482 = CARTESIAN_POINT ( 'NONE',  ( 56.65037692655918988, 51.89948385550241028, -2.184720259617163762 ) ) ;
#8483 = CARTESIAN_POINT ( 'NONE',  ( -3.436319922987618902, 2.634841920961291439, -3.531542292955721862 ) ) ;
#8484 = CARTESIAN_POINT ( 'NONE',  ( 55.71335778527780036, 54.90051614449765793, -1.832500667257213056 ) ) ;
#8485 = VECTOR ( 'NONE', #6481, 1000.000000000000000 ) ;
#8486 = CARTESIAN_POINT ( 'NONE',  ( -4.688877333428352223, -21.02685410450703074, 9.999999999999998224 ) ) ;
#8487 = CARTESIAN_POINT ( 'NONE',  ( 55.96859303347804371, 62.19948385550240744, 4.306917132069425946 ) ) ;
#8488 = CARTESIAN_POINT ( 'NONE',  ( 0.3126073911696427010, 4.041451884327382338, -6.521455134176256610E-17 ) ) ;
#8489 = CARTESIAN_POINT ( 'NONE',  ( 45.90387839640214196, 60.69948385550240033, 5.676469297603166098 ) ) ;
#8490 = ADVANCED_BREP_SHAPE_REPRESENTATION ( '', ( #10205, #430 ), #2855 ) ;
#8491 = ORIENTED_EDGE ( 'NONE', *, *, #6924, .T. ) ;
#8492 = EDGE_LOOP ( 'NONE', ( #211, #3182 ) ) ;
#8493 = DIRECTION ( 'NONE',  ( 0.000000000000000000, -0.000000000000000000, 1.000000000000000000 ) ) ;
#8494 = EDGE_CURVE ( 'NONE', #12356, #8346, #12508, .T. ) ;
#8495 = CIRCLE ( 'NONE', #1620, 5.000000000000000888 ) ;
#8496 = CARTESIAN_POINT ( 'NONE',  ( 0.000000000000000000, 0.000000000000000000, 0.000000000000000000 ) ) ;
#8497 = FACE_BOUND ( 'NONE', #10072, .T. ) ;
#8498 = LINE ( 'NONE', #9665, #1193 ) ;
#8499 = CARTESIAN_POINT ( 'NONE',  ( 45.90387839640214196, 46.69948385550240744, 5.676469297603166098 ) ) ;
#8500 = AXIS2_PLACEMENT_3D ( 'NONE', #4252, #984, #8470 ) ;
#8501 = CARTESIAN_POINT ( 'NONE',  ( 57.36023556966787851, 45.00051614449763804, 0.02388180880515038476 ) ) ;
#8502 = CARTESIAN_POINT ( 'NONE',  ( -7.499999999999923617, -32.99038105676662269, 9.000000000000000000 ) ) ;
#8503 = VECTOR ( 'NONE', #8298, 1000.000000000000000 ) ;
#8504 = CARTESIAN_POINT ( 'NONE',  ( 56.81924384183011512, 64.19948385550240744, 4.924951120819313743 ) ) ;
#8505 = DIRECTION ( 'NONE',  ( 0.000000000000000000, 0.000000000000000000, 1.000000000000000000 ) ) ;
#8506 = AXIS2_PLACEMENT_3D ( 'NONE', #2404, #5336, #6443 ) ;
#8507 = CARTESIAN_POINT ( 'NONE',  ( 56.81924384183011512, 56.19948385550240744, 4.924951120819313743 ) ) ;
#8508 = VERTEX_POINT ( 'NONE', #11681 ) ;
#8509 = ADVANCED_FACE ( 'NONE', ( #7415 ), #9474, .F. ) ;
#8510 = ORIENTED_EDGE ( 'NONE', *, *, #281, .T. ) ;
#8511 = EDGE_CURVE ( 'NONE', #4066, #12594, #1024, .T. ) ;
#8512 = DIRECTION ( 'NONE',  ( 0.000000000000000000, -0.5000000000000011102, -0.8660254037844379305 ) ) ;
#8513 = DIRECTION ( 'NONE',  ( -0.000000000000000000, -0.000000000000000000, 1.000000000000000000 ) ) ;
#8514 = CONICAL_SURFACE ( 'NONE', #10925, 2.055000000000000160, 0.7853981633974400633 ) ;
#8515 = DIRECTION ( 'NONE',  ( 0.000000000000000000, 0.000000000000000000, 1.000000000000000000 ) ) ;
#8516 = CARTESIAN_POINT ( 'NONE',  ( 55.08986747509849380, 51.20051614449766220, 3.727524721679155384 ) ) ;
#8517 = CARTESIAN_POINT ( 'NONE',  ( 54.13287192849671214, 60.70051614449766220, -5.649768623646139964 ) ) ;
#8518 = CARTESIAN_POINT ( 'NONE',  ( 57.61547081786812896, 46.09948385550240602, 2.450534656007040901 ) ) ;
#8519 = CARTESIAN_POINT ( 'NONE',  ( 10.00000000000000000, 15.00000000000001776, 9.999999999999998224 ) ) ;
#8520 = CARTESIAN_POINT ( 'NONE',  ( 45.27934281921082516, 55.70051614449766220, 6.458785618021089192 ) ) ;
#8521 = ORIENTED_EDGE ( 'NONE', *, *, #6133, .F. ) ;
#8522 = ORIENTED_EDGE ( 'NONE', *, *, #10484, .T. ) ;
#8523 = EDGE_LOOP ( 'NONE', ( #1557, #7776, #9095, #7112 ) ) ;
#8524 = FACE_OUTER_BOUND ( 'NONE', #12696, .T. ) ;
#8525 = CARTESIAN_POINT ( 'NONE',  ( 6.518095160331718319, 2.933089652807546077, -5.080260301817233426 ) ) ;
#8526 = DIRECTION ( 'NONE',  ( 0.000000000000000000, 0.000000000000000000, 1.000000000000000000 ) ) ;
#8527 = DIRECTION ( 'NONE',  ( -0.000000000000000000, 0.000000000000000000, -1.000000000000000000 ) ) ;
#8528 = DIRECTION ( 'NONE',  ( -1.000000000000000000, 0.000000000000000000, 0.000000000000000000 ) ) ;
#8529 = CARTESIAN_POINT ( 'NONE',  ( 44.88205777487398507, 49.19948385550240744, -3.688883143319540814 ) ) ;
#8530 = CARTESIAN_POINT ( 'NONE',  ( 52.29715082351547295, 62.39948385550240317, 6.992620115222774047 ) ) ;
#8531 = EDGE_CURVE ( 'NONE', #8295, #1117, #1770, .T. ) ;
#8532 = CARTESIAN_POINT ( 'NONE',  ( 54.72065718078918906, 44.70051614449765509, -6.458785618021089192 ) ) ;
#8533 = CIRCLE ( 'NONE', #2558, 2.396904916527700102 ) ;
#8534 = CARTESIAN_POINT ( 'NONE',  ( -2.649999999999988365, 15.00000000000001599, -9.999999999999998224 ) ) ;
#8535 = CARTESIAN_POINT ( 'NONE',  ( 5.991014884144048480, 4.330127018922193649, -2.499999999999998668 ) ) ;
#8536 = CARTESIAN_POINT ( 'NONE',  ( 54.13287192849671214, 58.70051614449765509, -5.649768623646139964 ) ) ;
#8537 = CARTESIAN_POINT ( 'NONE',  ( 44.28664221472220675, 59.09948385550240602, -1.832500667257165317 ) ) ;
#8538 = B_SPLINE_CURVE_WITH_KNOTS ( 'NONE', 3,
 ( #8297, #12362, #6019, #1990, #10429 ),
 .UNSPECIFIED., .F., .F.,
 ( 4, 1, 4 ),
 ( 0.000000000000000000, 0.002309401076758505356, 0.004618802153517010713 ),
 .UNSPECIFIED. ) ;
#8539 = DIRECTION ( 'NONE',  ( 0.000000000000000000, 0.000000000000000000, 1.000000000000000000 ) ) ;
#8540 = EDGE_CURVE ( 'NONE', #1320, #10107, #6648, .T. ) ;
#8541 = ORIENTED_EDGE ( 'NONE', *, *, #5197, .F. ) ;
#8542 = CARTESIAN_POINT ( 'NONE',  ( -62.49999999999997158, 32.50000000000001421, -9.999999999999998224 ) ) ;
#8543 = ORIENTED_EDGE ( 'NONE', *, *, #13177, .T. ) ;
#8544 = CARTESIAN_POINT ( 'NONE',  ( 53.50000000000000000, 4.475777889183788807E-16, -3.309499999999999886 ) ) ;
#8545 = DIRECTION ( 'NONE',  ( -1.000000000000000000, -0.000000000000000000, -0.000000000000000000 ) ) ;
#8546 = CARTESIAN_POINT ( 'NONE',  ( 4.124214193018076458, 2.028338413290941222, -3.513185186763556622 ) ) ;
#8547 = VECTOR ( 'NONE', #11277, 1000.000000000000000 ) ;
#8548 = CARTESIAN_POINT ( 'NONE',  ( 57.36023556966787851, 53.99948385550239038, -0.02388180880522424582 ) ) ;
#8549 = DIRECTION ( 'NONE',  ( -0.000000000000000000, -0.000000000000000000, 1.000000000000000000 ) ) ;
#8550 = CARTESIAN_POINT ( 'NONE',  ( 53.54508667620424234, 54.70051614449765509, -4.840751629271188961 ) ) ;
#8551 = LINE ( 'NONE', #4532, #49 ) ;
#8552 = B_SPLINE_CURVE_WITH_KNOTS ( 'NONE', 3,
 ( #5606, #12778, #9815, #13048 ),
 .UNSPECIFIED., .F., .F.,
 ( 4, 4 ),
 ( 2.380739282167303683E-07, 0.002044882221487525839 ),
 .UNSPECIFIED. ) ;
#8553 = CARTESIAN_POINT ( 'NONE',  ( 2.449293598294706513E-15, -20.00000000000000000, -9.000000000000000000 ) ) ;
#8554 = CARTESIAN_POINT ( 'NONE',  ( 45.86712807150323812, 61.29948385550240886, -5.649768623646098220 ) ) ;
#8555 = PLANE ( 'NONE',  #2485 ) ;
#8556 = ORIENTED_EDGE ( 'NONE', *, *, #13348, .T. ) ;
#8557 = ORIENTED_EDGE ( 'NONE', *, *, #8889, .T. ) ;
#8558 = ORIENTED_EDGE ( 'NONE', *, *, #7910, .T. ) ;
#8559 = DIRECTION ( 'NONE',  ( -1.000000000000000000, 0.000000000000000000, 0.000000000000000000 ) ) ;
#8560 = DIRECTION ( 'NONE',  ( 0.000000000000000000, 0.000000000000000000, -1.000000000000000000 ) ) ;
#8561 = CARTESIAN_POINT ( 'NONE',  ( 4.000000000000000000, 2.309401076758497151, -3.433295621305379353 ) ) ;
#8562 = CARTESIAN_POINT ( 'NONE',  ( 55.94051828345050836, 51.79948385550240175, -4.345558710429103577 ) ) ;
#8563 = CARTESIAN_POINT ( 'NONE',  ( 55.96859303347802239, 44.80051614449767072, -4.306917132069484566 ) ) ;
#8564 = FACE_OUTER_BOUND ( 'NONE', #8452, .T. ) ;
#8565 = CARTESIAN_POINT ( 'NONE',  ( 55.94051828345050836, 45.79948385550240886, -4.345558710429104465 ) ) ;
#8566 = EDGE_CURVE ( 'NONE', #10987, #12922, #6180, .T. ) ;
#8567 =( NAMED_UNIT ( * ) SI_UNIT ( $, .STERADIAN. ) SOLID_ANGLE_UNIT ( ) );
#8568 = EDGE_CURVE ( 'NONE', #1304, #13574, #9391, .T. ) ;
#8569 = CARTESIAN_POINT ( 'NONE',  ( 49.97728705011486738, 53.49948385550240459, -8.000000000000001776 ) ) ;
#8570 = EDGE_CURVE ( 'NONE', #4274, #13327, #7475, .T. ) ;
#8571 = ORIENTED_EDGE ( 'NONE', *, *, #2576, .T. ) ;
#8572 = VERTEX_POINT ( 'NONE', #12444 ) ;
#8573 = B_SPLINE_CURVE_WITH_KNOTS ( 'NONE', 3,
 ( #12058, #2439, #8950, #6606, #237, #4662 ),
 .UNSPECIFIED., .F., .F.,
 ( 4, 2, 4 ),
 ( 0.000000000000000000, 0.002086519881787259317, 0.004173039763574518633 ),
 .UNSPECIFIED. ) ;
#8574 = CARTESIAN_POINT ( 'NONE',  ( 8.500000000000000000, 0.000000000000000000, 7.900000000000002132 ) ) ;
#8575 = VECTOR ( 'NONE', #2698, 1000.000000000000000 ) ;
#8576 = LINE ( 'NONE', #4632, #5989 ) ;
#8577 = CARTESIAN_POINT ( 'NONE',  ( 44.91013252490150620, 50.20051614449766220, -3.727524721679154940 ) ) ;
#8578 = CARTESIAN_POINT ( 'NONE',  ( 43.33558569842706021, 61.90051614449766504, 2.141517661632167169 ) ) ;
#8579 = CARTESIAN_POINT ( 'NONE',  ( 43.18075615816989199, 47.19948385550240744, -4.924951120819313743 ) ) ;
#8580 = CARTESIAN_POINT ( 'NONE',  ( 18.00000000000000355, -20.00000000000000000, -12.00000000000000000 ) ) ;
#8581 = CARTESIAN_POINT ( 'NONE',  ( 57.61547081786810764, 54.90051614449765793, -2.450534656007114176 ) ) ;
#8582 = AXIS2_PLACEMENT_3D ( 'NONE', #3369, #2385, #6364 ) ;
#8583 = ORIENTED_EDGE ( 'NONE', *, *, #5956, .F. ) ;
#8584 = SHAPE_REPRESENTATION ( 'idle roller', ( #430 ), #11038 ) ;
#8585 = ORIENTED_EDGE ( 'NONE', *, *, #1775, .T. ) ;
#8586 = VERTEX_POINT ( 'NONE', #7277 ) ;
#8587 = EDGE_LOOP ( 'NONE', ( #4541, #1434, #12825, #8807 ) ) ;
#8588 = DIRECTION ( 'NONE',  ( -9.710251638871371392E-17, -5.969973981896233748E-17, -1.000000000000000000 ) ) ;
#8589 = EDGE_CURVE ( 'NONE', #3920, #13411, #8723, .T. ) ;
#8590 = DIRECTION ( 'NONE',  ( 0.000000000000000000, 0.000000000000000000, -1.000000000000000000 ) ) ;
#8591 = CARTESIAN_POINT ( 'NONE',  ( 0.3117969352650132309, 2.419842229202153305, -4.999999999999999112 ) ) ;
#8592 = DIRECTION ( 'NONE',  ( 1.000000000000000000, 3.469446951953615175E-16, 0.000000000000000000 ) ) ;
#8593 = CARTESIAN_POINT ( 'NONE',  ( 55.08986747509847248, 49.79948385550240175, -3.727524721679197572 ) ) ;
#8594 = DIRECTION ( 'NONE',  ( -0.000000000000000000, -0.000000000000000000, 1.000000000000000000 ) ) ;
#8595 = CARTESIAN_POINT ( 'NONE',  ( 45.31609314410960820, 46.30051614449766362, -6.485486291978072693 ) ) ;
#8596 = CIRCLE ( 'NONE', #9472, 4.000000000000000000 ) ;
#8597 = VECTOR ( 'NONE', #1385, 1000.000000000000000 ) ;
#8598 = DIRECTION ( 'NONE',  ( -0.000000000000000000, -0.000000000000000000, -1.000000000000000000 ) ) ;
#8599 = CARTESIAN_POINT ( 'NONE',  ( -7.499999999999998224, -20.00000000000000000, -20.00000000000000000 ) ) ;
#8600 = ADVANCED_FACE ( 'NONE', ( #1492 ), #9677, .T. ) ;
#8601 = CARTESIAN_POINT ( 'NONE',  ( 57.36023556966787851, 55.00051614449765225, 0.02388180880515038476 ) ) ;
#8602 = CARTESIAN_POINT ( 'NONE',  ( 43.69122665457040000, 56.99948385550241170, 0.02388180880521036456 ) ) ;
#8603 = EDGE_LOOP ( 'NONE', ( #3465, #3264, #10888, #4253 ) ) ;
#8604 = STYLED_ITEM ( 'NONE', ( #9582 ), #9629 ) ;
#8605 = AXIS2_PLACEMENT_3D ( 'NONE', #12430, #8229, #10498 ) ;
#8606 = CARTESIAN_POINT ( 'NONE',  ( 50.00000000000000000, 12.59655753109423237, 0.000000000000000000 ) ) ;
#8607 = ORIENTED_EDGE ( 'NONE', *, *, #5014, .T. ) ;
#8608 = CARTESIAN_POINT ( 'NONE',  ( 0.1217565302851100623, 3.710888496608919507, -0.5725525826504660465 ) ) ;
#8609 = EDGE_CURVE ( 'NONE', #10938, #4659, #12844, .T. ) ;
#8610 = PLANE ( 'NONE',  #4285 ) ;
#8611 = CARTESIAN_POINT ( 'NONE',  ( 4.158413352280813768, 2.044871626972823986, -3.541821552872968404 ) ) ;
#8612 =( NAMED_UNIT ( * ) PLANE_ANGLE_UNIT ( ) SI_UNIT ( $, .RADIAN. ) );
#8613 = CARTESIAN_POINT ( 'NONE',  ( 43.33558569842703179, 53.09948385550240602, -2.141517661632099223 ) ) ;
#8614 = PRODUCT_RELATED_PRODUCT_CATEGORY ( 'part', '', ( #11401 ) ) ;
#8615 = AXIS2_PLACEMENT_3D ( 'NONE', #10876, #12124, #6743 ) ;
#8616 = VECTOR ( 'NONE', #11386, 1000.000000000000000 ) ;
#8617 = CARTESIAN_POINT ( 'NONE',  ( 51.97223112728249816, 50.60051614449765367, -5.992620115222793586 ) ) ;
#8618 = DIRECTION ( 'NONE',  ( 0.000000000000000000, 0.000000000000000000, -1.000000000000000000 ) ) ;
#8619 = CARTESIAN_POINT ( 'NONE',  ( 2.682243648011666703, 3.070208061305304881, -0.04852650426601266831 ) ) ;
#8620 = CARTESIAN_POINT ( 'NONE',  ( 0.2174200650117547873, 3.876582599186211731, 0.2855619784720684895 ) ) ;
#8621 = CARTESIAN_POINT ( 'NONE',  ( 49.97728705011488159, 57.49948385550241170, -7.000000000000000888 ) ) ;
#8622 = DIRECTION ( 'NONE',  ( 1.000000000000000000, -9.251858538542972814E-17, 0.000000000000000000 ) ) ;
#8623 = ORIENTED_EDGE ( 'NONE', *, *, #5805, .F. ) ;
#8624 = EDGE_LOOP ( 'NONE', ( #1439, #8153, #1033, #2733 ) ) ;
#8625 = ORIENTED_EDGE ( 'NONE', *, *, #11002, .F. ) ;
#8626 = CARTESIAN_POINT ( 'NONE',  ( -4.999999999999998224, -20.00000000000000000, 15.00000000000000355 ) ) ;
#8627 = CARTESIAN_POINT ( 'NONE',  ( 4.211140560182196957, 2.431303136016536470, -3.745885042887433514 ) ) ;
#8628 = CARTESIAN_POINT ( 'NONE',  ( 20.00000000000000000, -20.00000000000000000, -23.00000000000000000 ) ) ;
#8629 = CARTESIAN_POINT ( 'NONE',  ( 0.3126073911695746443, -2.020725942163797750, -3.499999999999999556 ) ) ;
#8630 = CARTESIAN_POINT ( 'NONE',  ( 55.94051828345050836, 55.79948385550239465, -4.345558710429103577 ) ) ;
#8631 = CARTESIAN_POINT ( 'NONE',  ( 50.02271294988505446, 56.50051614449766646, -7.000000000000000888 ) ) ;
#8632 = CARTESIAN_POINT ( 'NONE',  ( 75.00000000000002842, -39.99999999999998579, 10.00000000000000000 ) ) ;
#8633 = EDGE_CURVE ( 'NONE', #7656, #9307, #6646, .T. ) ;
#8634 = CARTESIAN_POINT ( 'NONE',  ( 42.63976443033212860, 48.99948385550240459, 0.02388180880522514787 ) ) ;
#8635 = CARTESIAN_POINT ( 'NONE',  ( -17.85000000000000142, -19.99999999999999289, -23.00000000000000000 ) ) ;
#8636 = VECTOR ( 'NONE', #4704, 1000.000000000000000 ) ;
#8637 = CARTESIAN_POINT ( 'NONE',  ( 47.42335538002188144, 58.59948385550239891, 8.007379884777233059 ) ) ;
#8638 = EDGE_CURVE ( 'NONE', #844, #11042, #6774, .T. ) ;
#8639 = EDGE_LOOP ( 'NONE', ( #12841, #1186, #377, #11539, #6286, #3715, #11675, #5583, #11283 ) ) ;
#8640 = ORIENTED_EDGE ( 'NONE', *, *, #12523, .F. ) ;
#8641 = EDGE_CURVE ( 'NONE', #9009, #4571, #649, .T. ) ;
#8642 = CARTESIAN_POINT ( 'NONE',  ( 2.000000000000000000, -1.502314598737159426E-15, -1.535500000000000087 ) ) ;
#8643 = EDGE_CURVE ( 'NONE', #9556, #10373, #7086, .T. ) ;
#8644 = VECTOR ( 'NONE', #9644, 1000.000000000000000 ) ;
#8645 = EDGE_CURVE ( 'NONE', #9857, #12658, #1544, .T. ) ;
#8646 = CARTESIAN_POINT ( 'NONE',  ( 2.482347295856823136E-15, -20.00000000000000000, -8.999999999999996447 ) ) ;
#8647 = CARTESIAN_POINT ( 'NONE',  ( 48.02776887271750184, 57.60051614449765367, 5.992620115222795363 ) ) ;
#8648 = FACE_BOUND ( 'NONE', #133, .T. ) ;
#8649 = CARTESIAN_POINT ( 'NONE',  ( 43.18075615816989199, 49.19948385550240744, -4.924951120819313743 ) ) ;
#8650 = EDGE_CURVE ( 'NONE', #10627, #10076, #6854, .T. ) ;
#8651 = CARTESIAN_POINT ( 'NONE',  ( 4.033901012036116285, 2.321269032827693035, 2.979444097106929146 ) ) ;
#8652 = CARTESIAN_POINT ( 'NONE',  ( 54.72065718078918906, 56.70051614449766930, -6.458785618021089192 ) ) ;
#8653 = VECTOR ( 'NONE', #10665, 1000.000000000000114 ) ;
#8654 = PRODUCT_DEFINITION_SHAPE ( 'NONE', 'NONE',  #13674 ) ;
#8655 = CIRCLE ( 'NONE', #2025, 1.500000000000000222 ) ;
#8656 = CONICAL_SURFACE ( 'NONE', #11967, 2.500000000000000888, 0.9599310885968785900 ) ;
#8657 = VERTEX_POINT ( 'NONE', #6514 ) ;
#8658 = ORIENTED_EDGE ( 'NONE', *, *, #11285, .F. ) ;
#8659 = ORIENTED_EDGE ( 'NONE', *, *, #1300, .T. ) ;
#8660 = ORIENTED_EDGE ( 'NONE', *, *, #10529, .T. ) ;
#8661 = CARTESIAN_POINT ( 'NONE',  ( 0.5000000000000000000, -6.429618962271402616, -1.000000000000000000 ) ) ;
#8662 = CARTESIAN_POINT ( 'NONE',  ( -59.84999999999998721, 32.50000000000001421, 15.00000000000000178 ) ) ;
#8663 = CARTESIAN_POINT ( 'NONE',  ( 0.000000000000000000, 0.000000000000000000, -15.00000000000000000 ) ) ;
#8664 = DIRECTION ( 'NONE',  ( -1.000000000000000000, -0.000000000000000000, -0.000000000000000000 ) ) ;
#8665 = CARTESIAN_POINT ( 'NONE',  ( 2.000000000000005329, -3.464101615137751722, 0.000000000000000000 ) ) ;
#8666 = VECTOR ( 'NONE', #10536, 999.9999999999998863 ) ;
#8667 = CARTESIAN_POINT ( 'NONE',  ( 46.49166364869460466, 50.69948385550240744, 4.867452303228209765 ) ) ;
#8668 = VECTOR ( 'NONE', #23, 1000.000000000000000 ) ;
#8669 = CARTESIAN_POINT ( 'NONE',  ( 9.999999999999994671, 20.00000000000001421, -9.999999999999998224 ) ) ;
#8670 = CARTESIAN_POINT ( 'NONE',  ( 42.38452918213190657, 45.90051614449766504, 2.450534656007115508 ) ) ;
#8671 = LINE ( 'NONE', #7770, #6457 ) ;
#8672 = FACE_OUTER_BOUND ( 'NONE', #9685, .T. ) ;
#8673 = CARTESIAN_POINT ( 'NONE',  ( 50.02271294988505446, 58.50051614449765935, -7.000000000000000888 ) ) ;
#8674 = CARTESIAN_POINT ( 'NONE',  ( 44.28664221472220675, 63.09948385550240602, -1.832500667257165317 ) ) ;
#8675 = VERTEX_POINT ( 'NONE', #2267 ) ;
#8676 = DIRECTION ( 'NONE',  ( -1.000000000000000000, -4.082155997157843695E-16, 0.000000000000000000 ) ) ;
#8677 = VERTEX_POINT ( 'NONE', #4357 ) ;
#8678 = FACE_OUTER_BOUND ( 'NONE', #9918, .T. ) ;
#8679 = VECTOR ( 'NONE', #12654, 1000.000000000000000 ) ;
#8680 = EDGE_CURVE ( 'NONE', #1421, #5149, #10170, .T. ) ;
#8681 = CARTESIAN_POINT ( 'NONE',  ( 4.000000000000003553, 0.000000000000000000, 3.500000000000000000 ) ) ;
#8682 = CARTESIAN_POINT ( 'NONE',  ( 6.507056549636238252, 2.993353539201078828, 4.999999999999999112 ) ) ;
#8683 = FILL_AREA_STYLE ('',( #2307 ) ) ;
#8684 = CARTESIAN_POINT ( 'NONE',  ( 43.34962307344081012, 50.89948385550241028, 2.184720259617164650 ) ) ;
#8685 = CARTESIAN_POINT ( 'NONE',  ( 1.267864665261691752E-11, -20.00000000000000000, 9.999999999999998224 ) ) ;
#8686 = CARTESIAN_POINT ( 'NONE',  ( 44.91013252490150620, 60.20051614449766220, -3.727524721679154940 ) ) ;
#8687 = DIRECTION ( 'NONE',  ( -9.710251638871371392E-17, -5.969973981896233748E-17, -1.000000000000000000 ) ) ;
#8688 = DIRECTION ( 'NONE',  ( -1.000000000000000000, -0.000000000000000000, -0.000000000000000000 ) ) ;
#8689 = CARTESIAN_POINT ( 'NONE',  ( 8.500000000000000000, 0.000000000000000000, 0.000000000000000000 ) ) ;
#8690 = CARTESIAN_POINT ( 'NONE',  ( 54.09612160359786515, 59.69948385550240033, -5.676469297603166098 ) ) ;
#8691 = PLANE ( 'NONE',  #8907 ) ;
#8692 = VERTEX_POINT ( 'NONE', #7610 ) ;
#8693 = UNCERTAINTY_MEASURE_WITH_UNIT (LENGTH_MEASURE( 1.000000000000000082E-05 ), #6178, 'distance_accuracy_value', 'NONE');
#8694 = ORIENTED_EDGE ( 'NONE', *, *, #2641, .F. ) ;
#8695 = CARTESIAN_POINT ( 'NONE',  ( 50.00000000000000000, 40.00000000000000000, 0.000000000000000000 ) ) ;
#8696 = CARTESIAN_POINT ( 'NONE',  ( 1.250000000000000000, -6.429618962271402616, 0.000000000000000000 ) ) ;
#8697 = CARTESIAN_POINT ( 'NONE',  ( 4.086262629614032527, -4.082406995609991540, -0.07093633357110748494 ) ) ;
#8698 = DIRECTION ( 'NONE',  ( 0.5000000000000103251, -0.8660254037844327124, 0.000000000000000000 ) ) ;
#8699 = FACE_OUTER_BOUND ( 'NONE', #11659, .T. ) ;
#8700 = CARTESIAN_POINT ( 'NONE',  ( 56.66441430157296821, 54.09948385550240602, 2.141517661632100111 ) ) ;
#8701 = CARTESIAN_POINT ( 'NONE',  ( 54.09612160359792199, 55.30051614449765651, 5.676469297603124353 ) ) ;
#8702 = DIRECTION ( 'NONE',  ( -1.000000000000000000, 0.000000000000000000, 0.000000000000000000 ) ) ;
#8703 = EDGE_CURVE ( 'NONE', #5335, #3586, #8552, .T. ) ;
#8704 = CARTESIAN_POINT ( 'NONE',  ( 45.86712807150323812, 49.29948385550240175, -5.649768623646098220 ) ) ;
#8705 = DIRECTION ( 'NONE',  ( -0.000000000000000000, -0.000000000000000000, -1.000000000000000000 ) ) ;
#8706 = CARTESIAN_POINT ( 'NONE',  ( 41.58830220609386430, 62.99948385550241170, 0.02388180880523263147 ) ) ;
#8707 = B_SPLINE_CURVE_WITH_KNOTS ( 'NONE', 3,
 ( #2103, #8608, #1191, #12679 ),
 .UNSPECIFIED., .F., .F.,
 ( 4, 4 ),
 ( 2.380739282169052541E-07, 0.002044882221487534079 ),
 .UNSPECIFIED. ) ;
#8708 = EDGE_CURVE ( 'NONE', #10184, #11343, #8576, .T. ) ;
#8709 = AXIS2_PLACEMENT_3D ( 'NONE', #13284, #6126, #13560 ) ;
#8710 = ORIENTED_EDGE ( 'NONE', *, *, #12099, .T. ) ;
#8711 = ORIENTED_EDGE ( 'NONE', *, *, #3153, .T. ) ;
#8712 = ORIENTED_EDGE ( 'NONE', *, *, #12384, .F. ) ;
#8713 = LINE ( 'NONE', #6644, #10709 ) ;
#8714 = DIRECTION ( 'NONE',  ( -1.000000000000000000, -0.000000000000000000, -0.000000000000000000 ) ) ;
#8715 = CARTESIAN_POINT ( 'NONE',  ( 51.92680522751238925, 55.40051614449767214, 6.007379884777208190 ) ) ;
#8716 = CARTESIAN_POINT ( 'NONE',  ( -6.259644161404860030E-16, -4.618802153517027165, -3.433295621305388234 ) ) ;
#8717 = EDGE_CURVE ( 'NONE', #3891, #10160, #7540, .T. ) ;
#8718 = AXIS2_PLACEMENT_3D ( 'NONE', #3031, #13383, #3927 ) ;
#8719 = CARTESIAN_POINT ( 'NONE',  ( 42.39856655714566358, 52.89948385550241028, 2.493737253992119207 ) ) ;
#8720 = CARTESIAN_POINT ( 'NONE',  ( 44.03140696652192787, 59.19948385550238612, -4.306917132069425058 ) ) ;
#8721 = CARTESIAN_POINT ( 'NONE',  ( -74.99999999999998579, -7.500000000000027534, 10.00000000000000000 ) ) ;
#8722 = EDGE_CURVE ( 'NONE', #1223, #2588, #10714, .T. ) ;
#8723 = B_SPLINE_CURVE_WITH_KNOTS ( 'NONE', 3,
 ( #7208, #11413, #1933, #10376, #11487, #7815 ),
 .UNSPECIFIED., .F., .F.,
 ( 4, 2, 4 ),
 ( 0.002365888236227977302, 0.003551327329835078910, 0.004736766423442180518 ),
 .UNSPECIFIED. ) ;
#8724 = CIRCLE ( 'NONE', #2088, 5.000000000000000888 ) ;
#8725 = CARTESIAN_POINT ( 'NONE',  ( 50.02271294988505446, 60.50051614449766646, -8.000000000000001776 ) ) ;
#8726 = ADVANCED_FACE ( 'NONE', ( #1291, #11955 ), #1227, .T. ) ;
#8727 = ORIENTED_EDGE ( 'NONE', *, *, #10836, .F. ) ;
#8728 = ORIENTED_EDGE ( 'NONE', *, *, #4163, .F. ) ;
#8729 = ORIENTED_EDGE ( 'NONE', *, *, #8641, .T. ) ;
#8730 = VERTEX_POINT ( 'NONE', #8780 ) ;
#8731 = VECTOR ( 'NONE', #5394, 1000.000000000000000 ) ;
#8732 = FACE_OUTER_BOUND ( 'NONE', #8099, .T. ) ;
#8733 = FILL_AREA_STYLE_COLOUR ( '', #13408 ) ;
#8734 = FILL_AREA_STYLE_COLOUR ( '', #13458 ) ;
#8735 = DIRECTION ( 'NONE',  ( -9.858538378746663627E-23, 5.031452844637890958E-23, -1.000000000000000000 ) ) ;
#8736 = CARTESIAN_POINT ( 'NONE',  ( 0.1481481481481481122, -4.797713218419819903, -1.000000000000000000 ) ) ;
#8737 = CARTESIAN_POINT ( 'NONE',  ( 46.49166364869460466, 56.69948385550240744, 4.867452303228209765 ) ) ;
#8738 = CARTESIAN_POINT ( 'NONE',  ( 57.36023556966787851, 47.00051614449765935, 0.02388180880515038476 ) ) ;
#8739 = CARTESIAN_POINT ( 'NONE',  ( 57.60143344285435774, 51.10051614449766078, 2.493737253992045044 ) ) ;
#8740 = DIRECTION ( 'NONE',  ( -1.000000000000000000, -0.000000000000000000, -0.000000000000000000 ) ) ;
#8741 = DIRECTION ( 'NONE',  ( 0.000000000000000000, 0.000000000000000000, 1.000000000000000000 ) ) ;
#8742 = CARTESIAN_POINT ( 'NONE',  ( 50.02271294988505446, 54.50051614449765935, -7.000000000000000888 ) ) ;
#8743 = ORIENTED_EDGE ( 'NONE', *, *, #11147, .T. ) ;
#8744 = CARTESIAN_POINT ( 'NONE',  ( 2.548804901056335857E-15, 4.736522675502163437, -3.681124513963624612 ) ) ;
#8745 = ORIENTED_EDGE ( 'NONE', *, *, #2365, .F. ) ;
#8746 = CARTESIAN_POINT ( 'NONE',  ( -7.500000000000013323, -7.009618943233427935, -9.000000000000000000 ) ) ;
#8747 = DIRECTION ( 'NONE',  ( -1.000000000000000000, 0.000000000000000000, 0.000000000000000000 ) ) ;
#8748 = PLANE ( 'NONE',  #4239 ) ;
#8749 = CARTESIAN_POINT ( 'NONE',  ( 43.34962307344081012, 58.89948385550241028, 2.184720259617164650 ) ) ;
#8750 = DIRECTION ( 'NONE',  ( -1.000000000000000000, 0.000000000000000000, 0.000000000000000000 ) ) ;
#8751 = CARTESIAN_POINT ( 'NONE',  ( 51.92680522751238925, 55.40051614449767214, 6.007379884777208190 ) ) ;
#8752 = CARTESIAN_POINT ( 'NONE',  ( -62.49999999999997158, 32.50000000000001421, 15.00000000000000000 ) ) ;
#8753 = CARTESIAN_POINT ( 'NONE',  ( 1.267864665261691752E-11, -20.00000000000000000, 9.999999999999998224 ) ) ;
#8754 = ADVANCED_FACE ( 'NONE', ( #12028 ), #8418, .T. ) ;
#8755 = CARTESIAN_POINT ( 'NONE',  ( 6.385552186430389909, -5.773502691896263528, -1.564818079814629131E-31 ) ) ;
#8756 = CARTESIAN_POINT ( 'NONE',  ( 54.09612160359786515, 63.69948385550240744, -5.676469297603166098 ) ) ;
#8757 = CARTESIAN_POINT ( 'NONE',  ( 3.260336594487421635, -23.79080536174652494, 15.00000000000000355 ) ) ;
#8758 = ORIENTED_EDGE ( 'NONE', *, *, #12348, .F. ) ;
#8759 = ORIENTED_EDGE ( 'NONE', *, *, #9205, .F. ) ;
#8760 = VECTOR ( 'NONE', #1536, 999.9999999999998863 ) ;
#8761 = VERTEX_POINT ( 'NONE', #202 ) ;
#8762 = CARTESIAN_POINT ( 'NONE',  ( 4.175813232069147674, 2.061359961916367833, 3.570380186727398097 ) ) ;
#8763 = DIRECTION ( 'NONE',  ( 0.000000000000000000, 0.000000000000000000, -1.000000000000000000 ) ) ;
#8764 = DIRECTION ( 'NONE',  ( -9.710251638871371392E-17, -5.969973981896233748E-17, -1.000000000000000000 ) ) ;
#8765 = SURFACE_STYLE_FILL_AREA ( #9346 ) ;
#8766 = DIRECTION ( 'NONE',  ( 1.000000000000000000, 0.000000000000000000, 0.000000000000000000 ) ) ;
#8767 = FACE_BOUND ( 'NONE', #3399, .T. ) ;
#8768 = CARTESIAN_POINT ( 'NONE',  ( 56.66441430157296821, 52.09948385550240602, 2.141517661632100111 ) ) ;
#8769 = CARTESIAN_POINT ( 'NONE',  ( 55.96859303347802239, 52.80051614449764941, -4.306917132069484566 ) ) ;
#8770 = CARTESIAN_POINT ( 'NONE',  ( 10.00000000000000000, 15.00000000000001776, -15.00000000000000000 ) ) ;
#8771 = CARTESIAN_POINT ( 'NONE',  ( 43.34962307344081012, 50.89948385550241028, 2.184720259617164650 ) ) ;
#8772 = DIRECTION ( 'NONE',  ( 0.000000000000000000, -0.000000000000000000, 1.000000000000000000 ) ) ;
#8773 = CARTESIAN_POINT ( 'NONE',  ( 54.09612160359786515, 45.69948385550240744, -5.676469297603166098 ) ) ;
#8774 = ORIENTED_EDGE ( 'NONE', *, *, #6846, .T. ) ;
#8775 = VERTEX_POINT ( 'NONE', #4423 ) ;
#8776 = CARTESIAN_POINT ( 'NONE',  ( 0.000000000000000000, 0.8865213383406680414, -1.535500000000000975 ) ) ;
#8777 = ORIENTED_EDGE ( 'NONE', *, *, #6544, .F. ) ;
#8778 = CARTESIAN_POINT ( 'NONE',  ( -18.00000000000000355, -19.99999999999999289, -20.00000000000000000 ) ) ;
#8779 = EDGE_CURVE ( 'NONE', #940, #6987, #2336, .T. ) ;
#8780 = CARTESIAN_POINT ( 'NONE',  ( 2.000000000000000000, -0.8865213383406694847, 1.535500000000001419 ) ) ;
#8781 = CARTESIAN_POINT ( 'NONE',  ( 44.91013252490150620, 56.20051614449766220, -3.727524721679154940 ) ) ;
#8782 = DIRECTION ( 'NONE',  ( 0.000000000000000000, 0.000000000000000000, 1.000000000000000000 ) ) ;
#8783 = CARTESIAN_POINT ( 'NONE',  ( 54.72065718078924590, 50.29948385550240886, 6.458785618021043895 ) ) ;
#8784 = CARTESIAN_POINT ( 'NONE',  ( 52.29715082351547295, 56.39948385550238896, 6.992620115222774047 ) ) ;
#8785 = LINE ( 'NONE', #340, #4710 ) ;
#8786 = CARTESIAN_POINT ( 'NONE',  ( 41.58830220609386430, 62.00051614449766646, -0.02388180880514929535 ) ) ;
#8787 = VERTEX_POINT ( 'NONE', #9875 ) ;
#8788 = ORIENTED_EDGE ( 'NONE', *, *, #4899, .F. ) ;
#8789 = ORIENTED_EDGE ( 'NONE', *, *, #22, .F. ) ;
#8790 = MECHANICAL_DESIGN_GEOMETRIC_PRESENTATION_REPRESENTATION (  '', ( #9005 ), #4597 ) ;
#8791 = VERTEX_POINT ( 'NONE', #2759 ) ;
#8792 = LINE ( 'NONE', #3469, #9782 ) ;
#8793 =( NAMED_UNIT ( * ) PLANE_ANGLE_UNIT ( ) SI_UNIT ( $, .RADIAN. ) );
#8794 = LINE ( 'NONE', #6591, #10634 ) ;
#8795 = CARTESIAN_POINT ( 'NONE',  ( 6.080745460913608902, 0.5192545390863916310, 0.000000000000000000 ) ) ;
#8796 = CARTESIAN_POINT ( 'NONE',  ( 44.30067958973596376, 58.89948385550241028, 1.875703265242204099 ) ) ;
#8797 = CARTESIAN_POINT ( 'NONE',  ( 47.74827507625470702, 48.40051614449765793, -7.007379884777204637 ) ) ;
#8798 = CARTESIAN_POINT ( 'NONE',  ( 47.37792948025170858, 55.60051614449765367, 7.992620115222797139 ) ) ;
#8799 = AXIS2_PLACEMENT_3D ( 'NONE', #8695, #1004, #2117 ) ;
#8800 = DIRECTION ( 'NONE',  ( -3.469446951953611033E-15, 1.000000000000000000, 0.000000000000000000 ) ) ;
#8801 = LINE ( 'NONE', #2501, #2706 ) ;
#8802 = EDGE_CURVE ( 'NONE', #844, #5390, #2099, .T. ) ;
#8803 = CARTESIAN_POINT ( 'NONE',  ( 43.34962307344078880, 62.10051614449766078, -2.184720259617096705 ) ) ;
#8804 = MECHANICAL_DESIGN_GEOMETRIC_PRESENTATION_REPRESENTATION (  '', ( #397 ), #5062 ) ;
#8805 = ORIENTED_EDGE ( 'NONE', *, *, #8419, .T. ) ;
#8806 = CARTESIAN_POINT ( 'NONE',  ( 75.00000000000002842, -39.99999999999998579, 10.00000000000000000 ) ) ;
#8807 = ORIENTED_EDGE ( 'NONE', *, *, #10424, .F. ) ;
#8808 = CARTESIAN_POINT ( 'NONE',  ( 0.000000000000000000, 0.000000000000000000, 0.000000000000000000 ) ) ;
#8809 = CIRCLE ( 'NONE', #2392, 2.149999999999999023 ) ;
#8810 = FACE_OUTER_BOUND ( 'NONE', #2146, .T. ) ;
#8811 = CARTESIAN_POINT ( 'NONE',  ( 6.357987042335720318, 1.995285544161303992, 5.108766985362874102 ) ) ;
#8812 = EDGE_CURVE ( 'NONE', #1019, #7974, #7731, .T. ) ;
#8813 = CONICAL_SURFACE ( 'NONE', #9262, 3.500000000000000000, 1.047197551196600296 ) ;
#8814 = EDGE_CURVE ( 'NONE', #3281, #11826, #5949, .T. ) ;
#8815 = APPLICATION_PROTOCOL_DEFINITION ( 'draft international standard', 'automotive_design', 1998, #3366 ) ;
#8816 = CARTESIAN_POINT ( 'NONE',  ( 50.02271294988512551, 54.49948385550240459, 7.000000000000000888 ) ) ;
#8817 = CARTESIAN_POINT ( 'NONE',  ( 48.07319477248762496, 56.40051614449765793, -6.007379884777208190 ) ) ;
#8818 = CYLINDRICAL_SURFACE ( 'NONE', #11304, 2.649999999999985700 ) ;
#8819 = STYLED_ITEM ( 'NONE', ( #2811 ), #383 ) ;
#8820 = CARTESIAN_POINT ( 'NONE',  ( 7.336184427528458230, 9.926022037524705097E-16, 8.105212085995399107 ) ) ;
#8821 = CARTESIAN_POINT ( 'NONE',  ( 50.02271294988505446, 46.50051614449765935, -7.000000000000000888 ) ) ;
#8822 = CARTESIAN_POINT ( 'NONE',  ( 53.54508667620428497, 46.29948385550240886, 4.840751629271157874 ) ) ;
#8823 = LINE ( 'NONE', #8757, #5385 ) ;
#8824 = ORIENTED_EDGE ( 'NONE', *, *, #6072, .T. ) ;
#8825 = ORIENTED_EDGE ( 'NONE', *, *, #1021, .T. ) ;
#8826 = ADVANCED_BREP_SHAPE_REPRESENTATION ( '', ( #5714, #430 ), #9487 ) ;
#8827 = UNCERTAINTY_MEASURE_WITH_UNIT (LENGTH_MEASURE( 1.000000000000000082E-05 ), #63, 'distance_accuracy_value', 'NONE');
#8828 = ORIENTED_EDGE ( 'NONE', *, *, #9649, .F. ) ;
#8829 = FACE_OUTER_BOUND ( 'NONE', #7192, .T. ) ;
#8830 = CARTESIAN_POINT ( 'NONE',  ( -5.384454397937118664, 6.702023979852544604E-16, -5.000000000000000000 ) ) ;
#8831 = PRODUCT_DEFINITION_FORMATION_WITH_SPECIFIED_SOURCE ( 'ANY', '', #1011, .NOT_KNOWN. ) ;
#8832 = LINE ( 'NONE', #1546, #1110 ) ;
#8833 = EDGE_CURVE ( 'NONE', #6669, #5117, #121, .T. ) ;
#8834 = SURFACE_SIDE_STYLE ('',( #1616 ) ) ;
#8835 = CYLINDRICAL_SURFACE ( 'NONE', #9747, 12.50000000000000000 ) ;
#8836 = CARTESIAN_POINT ( 'NONE',  ( 4.082498951862918446, -2.020725942163685840, 3.500000000000002220 ) ) ;
#8837 = CARTESIAN_POINT ( 'NONE',  ( 52.25172492374527877, 53.40051614449765793, 7.007379884777203749 ) ) ;
#8838 = CARTESIAN_POINT ( 'NONE',  ( 0.000000000000000000, -0.8865213383406730374, -1.535499999999999421 ) ) ;
#8839 = CARTESIAN_POINT ( 'NONE',  ( 50.02271294988512551, 52.49948385550240459, 7.000000000000000888 ) ) ;
#8840 = CARTESIAN_POINT ( 'NONE',  ( 47.70284917648453415, 49.39948385550238896, -6.992620115222774047 ) ) ;
#8841 = EDGE_CURVE ( 'NONE', #5652, #5348, #1635, .T. ) ;
#8842 = CARTESIAN_POINT ( 'NONE',  ( 57.60143344285433642, 61.89948385550241738, -2.493737253992118319 ) ) ;
#8843 = PRESENTATION_LAYER_ASSIGNMENT (  '', '', ( #9502 ) ) ;
#8844 = AXIS2_PLACEMENT_3D ( 'NONE', #11668, #2192, #6436 ) ;
#8845 = EDGE_LOOP ( 'NONE', ( #13278, #3603, #5922, #11824 ) ) ;
#8846 = ORIENTED_EDGE ( 'NONE', *, *, #13238, .T. ) ;
#8847 = DIRECTION ( 'NONE',  ( 0.000000000000000000, 1.000000000000000000, 0.000000000000000000 ) ) ;
#8848 = ORIENTED_EDGE ( 'NONE', *, *, #4582, .T. ) ;
#8849 = CARTESIAN_POINT ( 'NONE',  ( 0.02993401039713550899, 2.688325911136453250, -2.343682934607766111 ) ) ;
#8850 = DIRECTION ( 'NONE',  ( 0.000000000000000000, 0.000000000000000000, 1.000000000000000000 ) ) ;
#8851 = CARTESIAN_POINT ( 'NONE',  ( 55.11794222512599362, 56.80051614449764941, -3.688883143319583446 ) ) ;
#8852 = AXIS2_PLACEMENT_3D ( 'NONE', #10027, #11202, #13468 ) ;
#8853 = CARTESIAN_POINT ( 'NONE',  ( 0.000000000000000000, -3.031088913245534755, -1.750000000000001332 ) ) ;
#8854 = CARTESIAN_POINT ( 'NONE',  ( 42.38452918213188525, 53.09948385550240602, -2.450534656007040013 ) ) ;
#8855 = CARTESIAN_POINT ( 'NONE',  ( 43.33558569842703179, 57.09948385550240602, -2.141517661632099223 ) ) ;
#8856 = CARTESIAN_POINT ( 'NONE',  ( -20.00000000000000000, -19.99999999999999289, -20.00000000000000000 ) ) ;
#8857 = CARTESIAN_POINT ( 'NONE',  ( 42.39856655714564226, 64.10051614449766078, -2.493737253992044156 ) ) ;
#8858 = EDGE_LOOP ( 'NONE', ( #148, #12235, #8100, #1840 ) ) ;
#8859 = AXIS2_PLACEMENT_3D ( 'NONE', #10961, #6694, #3504 ) ;
#8860 = ORIENTED_EDGE ( 'NONE', *, *, #4706, .T. ) ;
#8861 = ORIENTED_EDGE ( 'NONE', *, *, #5444, .T. ) ;
#8862 = ORIENTED_EDGE ( 'NONE', *, *, #2788, .T. ) ;
#8863 = CARTESIAN_POINT ( 'NONE',  ( 6.244004651191001898, 4.178905357954649347, -2.972460101650454156 ) ) ;
#8864 = DIRECTION ( 'NONE',  ( 0.5000000000000022204, 0.8660254037844374864, -0.000000000000000000 ) ) ;
#8865 = SURFACE_STYLE_FILL_AREA ( #5760 ) ;
#8866 = CARTESIAN_POINT ( 'NONE',  ( 6.534838248920897819, 2.951765777552412651, 5.112608298763836601 ) ) ;
#8867 = SURFACE_STYLE_FILL_AREA ( #3540 ) ;
#8868 = CARTESIAN_POINT ( 'NONE',  ( 55.11794222512601493, 56.19948385550240744, 3.688883143319541702 ) ) ;
#8869 = CARTESIAN_POINT ( 'NONE',  ( 49.97728705011495265, 47.50051614449766646, 7.000000000000000888 ) ) ;
#8870 = B_SPLINE_CURVE_WITH_KNOTS ( 'NONE', 3,
 ( #1509, #3607, #2559, #4645, #8863, #6790, #5756, #9957 ),
 .UNSPECIFIED., .F., .F.,
 ( 4, 2, 2, 4 ),
 ( 0.000000000000000000, 0.001493104274552340587, 0.002986208549104681607, 0.005972417098209364950 ),
 .UNSPECIFIED. ) ;
#8871 = CARTESIAN_POINT ( 'NONE',  ( 49.97728705011495265, 55.50051614449766646, 8.000000000000001776 ) ) ;
#8872 = AXIS2_PLACEMENT_3D ( 'NONE', #9891, #5622, #6792 ) ;
#8873 = CARTESIAN_POINT ( 'NONE',  ( -7.499999999999998224, -20.00000000000000000, -10.00000000000000000 ) ) ;
#8874=STYLED_ITEM('',(#13691),#5429);
#8875 = LINE ( 'NONE', #2708, #10656 ) ;
#8876 = CARTESIAN_POINT ( 'NONE',  ( 41.58830220609386430, 46.00051614449764514, -0.02388180880514929535 ) ) ;
#8877 = EDGE_LOOP ( 'NONE', ( #10983, #9659, #4644, #1119 ) ) ;
#8878 = CARTESIAN_POINT ( 'NONE',  ( -3.511755186886750479, 2.826662030176366081, -3.597382984111578086 ) ) ;
#8879 = ADVANCED_FACE ( 'NONE', ( #3795 ), #9742, .T. ) ;
#8880 = ORIENTED_EDGE ( 'NONE', *, *, #5195, .F. ) ;
#8881 = VECTOR ( 'NONE', #13194, 1000.000000000000000 ) ;
#8882 = AXIS2_PLACEMENT_3D ( 'NONE', #2956, #9517, #7324 ) ;
#8883 = FACE_OUTER_BOUND ( 'NONE', #12952, .T. ) ;
#8884 = AXIS2_PLACEMENT_3D ( 'NONE', #6682, #2312, #1258 ) ;
#8885 = CARTESIAN_POINT ( 'NONE',  ( 4.158806965674307854, -1.986429158307096321, -3.559403772175836256 ) ) ;
#8886 = DIRECTION ( 'NONE',  ( 1.000000000000000000, 0.000000000000000000, 0.000000000000000000 ) ) ;
#8887 = CARTESIAN_POINT ( 'NONE',  ( 50.02271294988512551, 60.49948385550240459, 7.000000000000000888 ) ) ;
#8888 = CARTESIAN_POINT ( 'NONE',  ( 55.69932041026405045, 57.10051614449766788, 1.875703265242156359 ) ) ;
#8889 = EDGE_CURVE ( 'NONE', #3906, #3300, #10009, .T. ) ;
#8890 = CARTESIAN_POINT ( 'NONE',  ( 4.175813232069148562, -2.061359961916374051, -3.570380186727397653 ) ) ;
#8891 = CARTESIAN_POINT ( 'NONE',  ( 14.00000000000000000, 1.610000000000000098, 0.000000000000000000 ) ) ;
#8892 = ADVANCED_FACE ( 'NONE', ( #4836 ), #4702, .F. ) ;
#8893 = CARTESIAN_POINT ( 'NONE',  ( 44.30067958973594955, 62.10051614449765367, -1.875703265242155693 ) ) ;
#8894 = CARTESIAN_POINT ( 'NONE',  ( 56.30877334542961421, 45.99948385550240459, -0.02388180880520959434 ) ) ;
#8895 = CIRCLE ( 'NONE', #1145, 1.499999999999998446 ) ;
#8896 = CARTESIAN_POINT ( 'NONE',  ( 5.599999999999999645, 2.020725942163688504, 3.500000000000000000 ) ) ;
#8897 = ADVANCED_FACE ( 'NONE', ( #3929 ), #3658, .F. ) ;
#8898 = ORIENTED_EDGE ( 'NONE', *, *, #1500, .T. ) ;
#8899 = AXIS2_PLACEMENT_3D ( 'NONE', #2429, #10674, #7840 ) ;
#8900 = ADVANCED_FACE ( 'NONE', ( #12364 ), #6980, .F. ) ;
#8901 = ORIENTED_EDGE ( 'NONE', *, *, #4185, .T. ) ;
#8902 = PLANE ( 'NONE',  #3719 ) ;
#8903 = CARTESIAN_POINT ( 'NONE',  ( 2.807080416178989513, -3.225969019225150003, -3.502507215260505014 ) ) ;
#8904 = CARTESIAN_POINT ( 'NONE',  ( 2.886521338340684917, 0.000000000000000000, 0.000000000000000000 ) ) ;
#8905 = CARTESIAN_POINT ( 'NONE',  ( 2.100000000000000089, 0.000000000000000000, -4.694516984716113228 ) ) ;
#8906 = CARTESIAN_POINT ( 'NONE',  ( 0.000000000000000000, 0.000000000000000000, -10.00000000000000000 ) ) ;
#8907 = AXIS2_PLACEMENT_3D ( 'NONE', #9855, #3566, #8622 ) ;
#8908 = CARTESIAN_POINT ( 'NONE',  ( 43.34962307344078880, 52.10051614449766078, -2.184720259617096705 ) ) ;
#8909 = CARTESIAN_POINT ( 'NONE',  ( 6.245813541929285506, 1.036329910265332499, -5.105320956836708390 ) ) ;
#8910 = DIRECTION ( 'NONE',  ( -0.000000000000000000, -0.000000000000000000, -1.000000000000000000 ) ) ;
#8911 = CARTESIAN_POINT ( 'NONE',  ( 47.74827507625478518, 50.59948385550238470, 7.007379884777227730 ) ) ;
#8912 = CARTESIAN_POINT ( 'NONE',  ( 57.61547081786812896, 60.09948385550240602, 2.450534656007040901 ) ) ;
#8913 = PRESENTATION_LAYER_ASSIGNMENT (  '', '', ( #70 ) ) ;
#8914 = EDGE_CURVE ( 'NONE', #8346, #844, #11335, .T. ) ;
#8915 = ORIENTED_EDGE ( 'NONE', *, *, #1702, .F. ) ;
#8916 = EDGE_LOOP ( 'NONE', ( #9595, #4713, #691 ) ) ;
#8917 = FACE_OUTER_BOUND ( 'NONE', #9217, .T. ) ;
#8918 = ORIENTED_EDGE ( 'NONE', *, *, #9478, .F. ) ;
#8919 = PLANE ( 'NONE',  #10260 ) ;
#8920 = B_SPLINE_CURVE_WITH_KNOTS ( 'NONE', 3,
 ( #13020, #6683, #6613, #2584, #10690, #5451, #6552, #7786 ),
 .UNSPECIFIED., .F., .F.,
 ( 4, 2, 2, 4 ),
 ( 0.000000000000000000, 0.001493104274552339720, 0.002986208549104679439, 0.005972417098209361480 ),
 .UNSPECIFIED. ) ;
#8921 = CARTESIAN_POINT ( 'NONE',  ( 4.050536630291688311, 2.401306687817038821, -2.976670123173768001 ) ) ;
#8922 = CARTESIAN_POINT ( 'NONE',  ( 46.49166364869456913, 52.30051614449766362, -4.867452303228181343 ) ) ;
#8923 = DIRECTION ( 'NONE',  ( 1.000000000000000000, 0.000000000000000000, 0.000000000000000000 ) ) ;
#8924 = CARTESIAN_POINT ( 'NONE',  ( 43.18075615816989199, 53.19948385550240744, -4.924951120819313743 ) ) ;
#8925 = CARTESIAN_POINT ( 'NONE',  ( 49.97728705011488159, 55.49948385550240459, -7.000000000000000888 ) ) ;
#8926 = CARTESIAN_POINT ( 'NONE',  ( 4.114405500665258231, -4.051151509359434577, 3.301207616706364010E-16 ) ) ;
#8927 = CIRCLE ( 'NONE', #12449, 1.500000000000000666 ) ;
#8928 = ADVANCED_FACE ( 'NONE', ( #10222 ), #4983, .T. ) ;
#8929 = CARTESIAN_POINT ( 'NONE',  ( 57.60143344285433642, 45.89948385550240317, -2.493737253992118319 ) ) ;
#8930 = ORIENTED_EDGE ( 'NONE', *, *, #2362, .F. ) ;
#8931 = VERTEX_POINT ( 'NONE', #7260 ) ;
#8932 = ORIENTED_EDGE ( 'NONE', *, *, #9417, .F. ) ;
#8933 = ORIENTED_EDGE ( 'NONE', *, *, #5617, .T. ) ;
#8934 = CARTESIAN_POINT ( 'NONE',  ( 2.449293598294706513E-15, -20.00000000000000000, -50.00000000000000000 ) ) ;
#8935 = AXIS2_PLACEMENT_3D ( 'NONE', #6059, #1950, #902 ) ;
#8936 = CARTESIAN_POINT ( 'NONE',  ( -2.000000000000000000, -6.429618962271402616, -1.000000000000000000 ) ) ;
#8937 = CYLINDRICAL_SURFACE ( 'NONE', #4782, 12.50000000000000000 ) ;
#8938 = CARTESIAN_POINT ( 'NONE',  ( 43.69122665457040000, 56.99948385550241170, 0.02388180880521036456 ) ) ;
#8939 = CARTESIAN_POINT ( 'NONE',  ( 47.70284917648459810, 47.60051614449766078, 6.992620115222797139 ) ) ;
#8940 = VECTOR ( 'NONE', #11300, 1000.000000000000000 ) ;
#8941 = CARTESIAN_POINT ( 'NONE',  ( 57.61547081786810764, 52.90051614449766504, -2.450534656007114176 ) ) ;
#8942 = CARTESIAN_POINT ( 'NONE',  ( -14.99999999999999645, -20.00000000000005329, -9.000000000000000000 ) ) ;
#8943 = CARTESIAN_POINT ( 'NONE',  ( 30.00000000000000000, -7.499999999999971578, -10.00000000000000000 ) ) ;
#8944 = CARTESIAN_POINT ( 'NONE',  ( 47.42335538002180328, 46.40051614449765793, -8.007379884777206414 ) ) ;
#8945 = CIRCLE ( 'NONE', #9818, 2.500000000000000888 ) ;
#8946 = EDGE_LOOP ( 'NONE', ( #7257, #2416, #3126, #10540 ) ) ;
#8947 = CARTESIAN_POINT ( 'NONE',  ( 1.925929944387235853E-31, 15.00000000000001599, -9.000000000000000000 ) ) ;
#8948 = EDGE_LOOP ( 'NONE', ( #1372, #10871, #10922, #1455, #7255 ) ) ;
#8949 = LINE ( 'NONE', #491, #8045 ) ;
#8950 = CARTESIAN_POINT ( 'NONE',  ( 3.972709601346592123, 3.429395227388311262, 1.191688283765307332 ) ) ;
#8951 = CARTESIAN_POINT ( 'NONE',  ( 44.03140696652192787, 57.19948385550238612, -4.306917132069425058 ) ) ;
#8952 = CIRCLE ( 'NONE', #9587, 1.500000000000001332 ) ;
#8953 = CARTESIAN_POINT ( 'NONE',  ( 50.02271294988506156, 58.50051614449765225, -6.000000000000000888 ) ) ;
#8954 = DIRECTION ( 'NONE',  ( -0.000000000000000000, -0.000000000000000000, -1.000000000000000000 ) ) ;
#8955 = FACE_OUTER_BOUND ( 'NONE', #3656, .T. ) ;
#8956 = CARTESIAN_POINT ( 'NONE',  ( 47.70284917648459100, 47.60051614449763946, 6.992620115222796251 ) ) ;
#8957 = CARTESIAN_POINT ( 'NONE',  ( 49.97728705011488159, 65.49948385550240459, -7.000000000000000888 ) ) ;
#8958 = DIRECTION ( 'NONE',  ( 0.000000000000000000, 0.000000000000000000, 1.000000000000000000 ) ) ;
#8959 = ORIENTED_EDGE ( 'NONE', *, *, #6297, .T. ) ;
#8960 = UNCERTAINTY_MEASURE_WITH_UNIT (LENGTH_MEASURE( 1.000000000000000082E-05 ), #2560, 'distance_accuracy_value', 'NONE');
#8961 = ORIENTED_EDGE ( 'NONE', *, *, #4265, .F. ) ;
#8962 = DIRECTION ( 'NONE',  ( 0.000000000000000000, 0.000000000000000000, 1.000000000000000000 ) ) ;
#8963 = CARTESIAN_POINT ( 'NONE',  ( 4.211140560182196957, -2.431303136016555122, -3.745885042887436622 ) ) ;
#8964 = LINE ( 'NONE', #3576, #5337 ) ;
#8965 = PRESENTATION_STYLE_ASSIGNMENT (( #4682 ) ) ;
#8966 = CARTESIAN_POINT ( 'NONE',  ( 6.541171661047875396, 2.934678558896536504, 5.142480235691129664 ) ) ;
#8967 = CARTESIAN_POINT ( 'NONE',  ( -75.00000000000001421, -2.602085213965211904E-14, 0.000000000000000000 ) ) ;
#8968 = CARTESIAN_POINT ( 'NONE',  ( 52.29715082351538769, 58.60051614449766078, -6.992620115222796251 ) ) ;
#8969 = DIRECTION ( 'NONE',  ( 0.000000000000000000, 1.000000000000000000, 0.000000000000000000 ) ) ;
#8970 = DIRECTION ( 'NONE',  ( -1.000000000000000000, 0.000000000000000000, 0.000000000000000000 ) ) ;
#8971 = CARTESIAN_POINT ( 'NONE',  ( 56.66441430157296821, 60.09948385550240602, 2.141517661632100111 ) ) ;
#8972 = CARTESIAN_POINT ( 'NONE',  ( 49.97728705011488159, 47.49948385550240459, -7.000000000000000888 ) ) ;
#8973 = CIRCLE ( 'NONE', #7874, 6.080745460913608902 ) ;
#8974 = CARTESIAN_POINT ( 'NONE',  ( 57.60143344285433642, 59.89948385550240317, -2.493737253992118319 ) ) ;
#8975 = ORIENTED_EDGE ( 'NONE', *, *, #3811, .T. ) ;
#8976 = VERTEX_POINT ( 'NONE', #6304 ) ;
#8977 = LINE ( 'NONE', #11950, #1052 ) ;
#8978 = ORIENTED_EDGE ( 'NONE', *, *, #3454, .F. ) ;
#8979 = LINE ( 'NONE', #12025, #9397 ) ;
#8980 = CARTESIAN_POINT ( 'NONE',  ( 6.534533895392296010, -2.951347675328743314, -5.111884124469654900 ) ) ;
#8981 = ADVANCED_FACE ( 'NONE', ( #9460 ), #1993, .F. ) ;
#8982 = CARTESIAN_POINT ( 'NONE',  ( 56.30877334542961421, 59.00051614449766646, 0.02388180880515774693 ) ) ;
#8983 = EDGE_CURVE ( 'NONE', #11359, #3701, #945, .T. ) ;
#8984 = CARTESIAN_POINT ( 'NONE',  ( 0.3126073911696399255, 2.020725942163686284, -3.499999999999999556 ) ) ;
#8985 = CARTESIAN_POINT ( 'NONE',  ( 57.61547081786812896, 52.09948385550241312, 2.450534656007040901 ) ) ;
#8986 = ADVANCED_FACE ( 'NONE', ( #12638 ), #9261, .F. ) ;
#8987 = CARTESIAN_POINT ( 'NONE',  ( 45.86712807150323812, 57.29948385550240175, -5.649768623646098220 ) ) ;
#8988 = CARTESIAN_POINT ( 'NONE',  ( 6.196878017913833858, -1.924500897298759172, -5.000000000000000888 ) ) ;
#8989 = CARTESIAN_POINT ( 'NONE',  ( 43.18075615816994173, 61.80051614449766362, 4.924951120819380357 ) ) ;
#8990 = EDGE_LOOP ( 'NONE', ( #6722, #3521, #2080, #10785 ) ) ;
#8991 = CONTEXT_DEPENDENT_SHAPE_REPRESENTATION ( #5417, #8654 ) ;
#8992 = ORIENTED_EDGE ( 'NONE', *, *, #4506, .F. ) ;
#8993 = ORIENTED_EDGE ( 'NONE', *, *, #13414, .F. ) ;
#8994 = ORIENTED_EDGE ( 'NONE', *, *, #5197, .T. ) ;
#8995 = CARTESIAN_POINT ( 'NONE',  ( 0.000000000000000000, -0.8865213383406694847, 1.535500000000001419 ) ) ;
#8996 = DIRECTION ( 'NONE',  ( -0.000000000000000000, 1.000000000000000000, -0.000000000000000000 ) ) ;
#8997 = LINE ( 'NONE', #9277, #10618 ) ;
#8998 = CARTESIAN_POINT ( 'NONE',  ( -13.67449106481168997, -13.83491329190049690, 0.000000000000000000 ) ) ;
#8999 = CARTESIAN_POINT ( 'NONE',  ( 43.69122665457040000, 54.99948385550239749, 0.02388180880521036456 ) ) ;
#9000 = CARTESIAN_POINT ( 'NONE',  ( 45.90387839640208512, 54.30051614449765651, -5.676469297603124353 ) ) ;
#9001 = CARTESIAN_POINT ( 'NONE',  ( 50.02271294988505446, 50.50051614449765935, -8.000000000000001776 ) ) ;
#9002 = CARTESIAN_POINT ( 'NONE',  ( 0.000000000000000000, 3.755786496842903495E-16, 3.500000000000000000 ) ) ;
#9003 = CARTESIAN_POINT ( 'NONE',  ( -74.99999999999998579, -7.500000000000027534, -10.00000000000000000 ) ) ;
#9004 = CARTESIAN_POINT ( 'NONE',  ( 58.41169779390614281, 45.00051614449765225, 0.02388180880515032231 ) ) ;
#9005=STYLED_ITEM('',(#13705),#10205);
#9006 = VERTEX_POINT ( 'NONE', #1920 ) ;
#9007 = EDGE_CURVE ( 'NONE', #7378, #3939, #8363, .T. ) ;
#9008 = DIRECTION ( 'NONE',  ( 0.000000000000000000, 0.000000000000000000, 1.000000000000000000 ) ) ;
#9009 = VERTEX_POINT ( 'NONE', #10562 ) ;
#9010 = DIRECTION ( 'NONE',  ( 0.000000000000000000, 0.000000000000000000, 1.000000000000000000 ) ) ;
#9011 = LINE ( 'NONE', #7979, #47 ) ;
#9012 = APPLICATION_PROTOCOL_DEFINITION ( 'draft international standard', 'automotive_design', 1998, #3103 ) ;
#9013 = CARTESIAN_POINT ( 'NONE',  ( 54.13287192849676188, 58.29948385550240175, 5.649768623646098220 ) ) ;
#9014 = VECTOR ( 'NONE', #7745, 1000.000000000000000 ) ;
#9015 = CARTESIAN_POINT ( 'NONE',  ( 55.94051828345050836, 49.79948385550240175, -4.345558710429103577 ) ) ;
#9016 = EDGE_CURVE ( 'NONE', #11826, #1384, #13220, .T. ) ;
#9017 = EDGE_CURVE ( 'NONE', #725, #5739, #9554, .T. ) ;
#9018 = CARTESIAN_POINT ( 'NONE',  ( 1.250000000000000000, -6.429618962271402616, 0.000000000000000000 ) ) ;
#9019 = DIRECTION ( 'NONE',  ( 0.000000000000000000, -0.4999999999999989453, 0.8660254037844391517 ) ) ;
#9020 = DIRECTION ( 'NONE',  ( -0.000000000000000000, 1.345283343056720273E-15, 1.000000000000000000 ) ) ;
#9021 = CARTESIAN_POINT ( 'NONE',  ( 57.36023556966787851, 47.00051614449764514, 0.02388180880515038476 ) ) ;
#9022 = CARTESIAN_POINT ( 'NONE',  ( 55.11794222512601493, 46.19948385550240744, 3.688883143319541702 ) ) ;
#9023 = DIRECTION ( 'NONE',  ( 1.000000000000000000, 0.000000000000000000, 0.000000000000000000 ) ) ;
#9024 = ORIENTED_EDGE ( 'NONE', *, *, #7701, .T. ) ;
#9025 = AXIS2_PLACEMENT_3D ( 'NONE', #5101, #1971, #3841 ) ;
#9026 = EDGE_LOOP ( 'NONE', ( #389, #474 ) ) ;
#9027 = EDGE_LOOP ( 'NONE', ( #7743, #150 ) ) ;
#9028 = CARTESIAN_POINT ( 'NONE',  ( 5.599999999999999645, -4.041451884327386779, 0.000000000000000000 ) ) ;
#9029 = PRODUCT_RELATED_PRODUCT_CATEGORY ( 'part', '', ( #12721 ) ) ;
#9030 = CARTESIAN_POINT ( 'NONE',  ( -3.309651814758565180, -5.455921364805393026, -1.000000000000000000 ) ) ;
#9031 = CARTESIAN_POINT ( 'NONE',  ( 4.050480423730738799, 1.376911654797411400, -3.567926555162023394 ) ) ;
#9032 = CARTESIAN_POINT ( 'NONE',  ( 0.000000000000000000, 0.000000000000000000, 0.000000000000000000 ) ) ;
#9033 = FACE_OUTER_BOUND ( 'NONE', #11461, .T. ) ;
#9034 = CARTESIAN_POINT ( 'NONE',  ( 45.86712807150329496, 57.70051614449765509, 5.649768623646139964 ) ) ;
#9035 = CONICAL_SURFACE ( 'NONE', #8383, 4.000000000000000000, 0.8911886515913786111 ) ;
#9036 = CARTESIAN_POINT ( 'NONE',  ( 6.092460485788117275, -1.005982284679170391, -5.000000000000000000 ) ) ;
#9037 = CARTESIAN_POINT ( 'NONE',  ( 0.000000000000000000, 0.5192545390863916310, -1.000000000000000000 ) ) ;
#9038 = CARTESIAN_POINT ( 'NONE',  ( 57.36023556966787851, 59.99948385550240459, -0.02388180880522424582 ) ) ;
#9039 = CARTESIAN_POINT ( 'NONE',  ( 56.65037692655918988, 47.89948385550240317, -2.184720259617163762 ) ) ;
#9040 = AXIS2_PLACEMENT_3D ( 'NONE', #3280, #8676, #7775 ) ;
#9041 = CARTESIAN_POINT ( 'NONE',  ( 50.02271294988512551, 48.49948385550240459, 7.000000000000000888 ) ) ;
#9042 = VERTEX_POINT ( 'NONE', #5489 ) ;
#9043 = VERTEX_POINT ( 'NONE', #12536 ) ;
#9044 = CARTESIAN_POINT ( 'NONE',  ( 3.878104551856474735, -0.7018542299754126912, -3.499999999999999556 ) ) ;
#9045 = VECTOR ( 'NONE', #10776, 1000.000000000000000 ) ;
#9046 = ORIENTED_EDGE ( 'NONE', *, *, #4811, .T. ) ;
#9047 = EDGE_CURVE ( 'NONE', #13190, #345, #11254, .T. ) ;
#9048 = FACE_OUTER_BOUND ( 'NONE', #6707, .T. ) ;
#9049 = VECTOR ( 'NONE', #12119, 1000.000000000000000 ) ;
#9050 = CARTESIAN_POINT ( 'NONE',  ( 4.175813232069148562, 4.122719923832741884, -2.765695189283172261E-17 ) ) ;
#9051 = CARTESIAN_POINT ( 'NONE',  ( 53.50833635130544508, 59.30051614449766362, 4.867452303228181343 ) ) ;
#9052 = CARTESIAN_POINT ( 'NONE',  ( 4.204115023516791005, -1.660442669500199919, -3.602151381774560068 ) ) ;
#9053 = CARTESIAN_POINT ( 'NONE',  ( 43.18075615816989199, 61.19948385550241454, -4.924951120819313743 ) ) ;
#9054 = CIRCLE ( 'NONE', #638, 12.50000000000000000 ) ;
#9055 = CARTESIAN_POINT ( 'NONE',  ( 47.74827507625478518, 64.59948385550239891, 7.007379884777227730 ) ) ;
#9056 = CARTESIAN_POINT ( 'NONE',  ( -4.101948962585906244, 2.368261337751074169, -3.681124513963621503 ) ) ;
#9057 = EDGE_CURVE ( 'NONE', #7909, #9204, #12730, .T. ) ;
#9058 = CARTESIAN_POINT ( 'NONE',  ( 57.61547081786812896, 52.09948385550241312, 2.450534656007040901 ) ) ;
#9059 = EDGE_CURVE ( 'NONE', #11058, #9006, #942, .T. ) ;
#9060 = VERTEX_POINT ( 'NONE', #2222 ) ;
#9061 = EDGE_CURVE ( 'NONE', #1857, #2067, #2091, .T. ) ;
#9062 = ORIENTED_EDGE ( 'NONE', *, *, #3625, .T. ) ;
#9063 = EDGE_CURVE ( 'NONE', #1386, #9183, #1976, .T. ) ;
#9064 = ORIENTED_EDGE ( 'NONE', *, *, #10658, .T. ) ;
#9065 = EDGE_LOOP ( 'NONE', ( #313, #6958, #7705, #6188 ) ) ;
#9066 = DIRECTION ( 'NONE',  ( 0.000000000000000000, 0.000000000000000000, 1.000000000000000000 ) ) ;
#9067 = AXIS2_PLACEMENT_3D ( 'NONE', #15, #4237, #6397 ) ;
#9068 = CARTESIAN_POINT ( 'NONE',  ( 20.00000000000000000, -14.99999999999999289, -23.00000000000000000 ) ) ;
#9069 = CARTESIAN_POINT ( 'NONE',  ( 12.17636723815371447, -11.24008670809939581, 0.000000000000000000 ) ) ;
#9070 = LINE ( 'NONE', #12309, #12153 ) ;
#9071 = ADVANCED_FACE ( 'NONE', ( #12798 ), #2288, .F. ) ;
#9072 = CARTESIAN_POINT ( 'NONE',  ( 30.00000000000000000, 1.040834085586084888E-14, 0.000000000000000000 ) ) ;
#9073 = CARTESIAN_POINT ( 'NONE',  ( 56.30877334542961421, 61.99948385550241170, -0.02388180880520959434 ) ) ;
#9074 = CARTESIAN_POINT ( 'NONE',  ( 55.94051828345054389, 55.20051614449766220, 4.345558710429044957 ) ) ;
#9075 = CARTESIAN_POINT ( 'NONE',  ( 42.39856655714564226, 62.10051614449765367, -2.493737253992044156 ) ) ;
#9076 = CARTESIAN_POINT ( 'NONE',  ( 45.15499999999999403, 0.000000000000000000, 0.000000000000000000 ) ) ;
#9077 = CARTESIAN_POINT ( 'NONE',  ( -74.99999999999998579, -2.602085213965210642E-14, 0.000000000000000000 ) ) ;
#9078 = CARTESIAN_POINT ( 'NONE',  ( 54.09612160359792199, 61.30051614449766362, 5.676469297603124353 ) ) ;
#9080 = VERTEX_POINT ( 'NONE', #2026 ) ;
#9079 = ORIENTED_EDGE ( 'NONE', *, *, #5389, .F. ) ;
#9081 = EDGE_CURVE ( 'NONE', #568, #3385, #3744, .T. ) ;
#9082 = CARTESIAN_POINT ( 'NONE',  ( -0.6448876103708541807, -4.246476118072358474, -0.2256878752776773356 ) ) ;
#9083 = EDGE_CURVE ( 'NONE', #11777, #9824, #9490, .T. ) ;
#9084 = ORIENTED_EDGE ( 'NONE', *, *, #13028, .F. ) ;
#9085 = CARTESIAN_POINT ( 'NONE',  ( 5.599999999999998757, 0.000000000000000000, 5.200000000000001066 ) ) ;
#9086 = FACE_OUTER_BOUND ( 'NONE', #6882, .T. ) ;
#9087 = CARTESIAN_POINT ( 'NONE',  ( 52.25172492374522903, 61.59948385550239891, -7.007379884777225953 ) ) ;
#9088 = CARTESIAN_POINT ( 'NONE',  ( 47.74827507625477807, 60.59948385550239891, 7.007379884777229506 ) ) ;
#9089 = CARTESIAN_POINT ( 'NONE',  ( -3.999999999999999112, 1.539600717838996324, -3.300726591567078039 ) ) ;
#9090 = CARTESIAN_POINT ( 'NONE',  ( -6.473970235329672780E-16, -4.862606272033106691, -3.745885042887442395 ) ) ;
#9091 = DIRECTION ( 'NONE',  ( 0.000000000000000000, 0.000000000000000000, 1.000000000000000000 ) ) ;
#9092 = CARTESIAN_POINT ( 'NONE',  ( 50.02271294988506156, 64.50051614449766646, -6.000000000000000888 ) ) ;
#9093 = CARTESIAN_POINT ( 'NONE',  ( 44.88205777487398507, 51.19948385550240744, -3.688883143319540814 ) ) ;
#9094 = DIRECTION ( 'NONE',  ( 0.000000000000000000, 0.000000000000000000, 1.000000000000000000 ) ) ;
#9095 = ORIENTED_EDGE ( 'NONE', *, *, #13072, .T. ) ;
#9096 = AXIS2_PLACEMENT_3D ( 'NONE', #2858, #765, #2022 ) ;
#9097 = EDGE_CURVE ( 'NONE', #6230, #3838, #4195, .T. ) ;
#9098 = CIRCLE ( 'NONE', #1790, 5.000000000000000888 ) ;
#9099 = AXIS2_PLACEMENT_3D ( 'NONE', #6967, #12145, #11938 ) ;
#9100 = ORIENTED_EDGE ( 'NONE', *, *, #1091, .T. ) ;
#9101 = ORIENTED_EDGE ( 'NONE', *, *, #3742, .T. ) ;
#9102 = CARTESIAN_POINT ( 'NONE',  ( 8.500000000000000000, 9.800365875394399578E-16, -7.900000000000002132 ) ) ;
#9103 = CARTESIAN_POINT ( 'NONE',  ( 6.245824673233021151, 4.939548505212935758, -1.655093584846096366 ) ) ;
#9104 = CARTESIAN_POINT ( 'NONE',  ( 6.242800618755285136, -4.918813924287352535, -1.690830708135802052 ) ) ;
#9105 = DIRECTION ( 'NONE',  ( 0.000000000000000000, -1.000000000000000000, 9.783878858594328898E-16 ) ) ;
#9106 = FACE_OUTER_BOUND ( 'NONE', #11380, .T. ) ;
#9107 = AXIS2_PLACEMENT_3D ( 'NONE', #11201, #13264, #7063 ) ;
#9108 = CARTESIAN_POINT ( 'NONE',  ( 44.03140696652198471, 61.80051614449767072, 4.306917132069485454 ) ) ;
#9109 = CARTESIAN_POINT ( 'NONE',  ( 1.753358200816401209E-16, -0.4883827417527520920, -4.999999999999999112 ) ) ;
#9110 = CARTESIAN_POINT ( 'NONE',  ( 55.08986747509847248, 63.79948385550241596, -3.727524721679197572 ) ) ;
#9111 = CARTESIAN_POINT ( 'NONE',  ( 4.000000000000000000, -2.309401076758514915, -5.000000000000000000 ) ) ;
#9112 = CARTESIAN_POINT ( 'NONE',  ( 47.70284917648453415, 61.39948385550241738, -6.992620115222774047 ) ) ;
#9113 = CARTESIAN_POINT ( 'NONE',  ( 50.02271294988512551, 52.49948385550240459, 7.000000000000000888 ) ) ;
#9114 =( BOUNDED_SURFACE ( )  B_SPLINE_SURFACE ( 3, 2, ( 
 ( #8233, #3722, #2761 ),
 ( #2829, #6840, #9052 ),
 ( #732, #4912, #5882 ),
 ( #13317, #9125, #5054 ),
 ( #3865, #12366, #8092 ),
 ( #12297, #1567, #7124 ) ),
 .UNSPECIFIED., .F., .F., .T. ) 
 B_SPLINE_SURFACE_WITH_KNOTS ( ( 4, 2, 4 ),
 ( 3, 3 ),
 ( 0.02027065861071770947, 0.02273072267836921331, 0.02519078674602071716 ),
 ( 0.000000000000000000, 1.000000000000000000 ),
 .UNSPECIFIED. ) 
 GEOMETRIC_REPRESENTATION_ITEM ( )  RATIONAL_B_SPLINE_SURFACE ( (
 ( 1.000000000000000000, 0.8047781708337304885, 1.000000000000000000),
 ( 1.000000000000000000, 0.8123765190705307671, 1.000000000000000000),
 ( 1.000000000000000000, 0.8190656277163975707, 1.000000000000000000),
 ( 1.000000000000000000, 0.8192366903512159348, 1.000000000000000000),
 ( 1.000000000000000000, 0.8126138454302893610, 1.000000000000000000),
 ( 1.000000000000000000, 0.8047712246031417660, 1.000000000000000000) ) ) 
 REPRESENTATION_ITEM ( '' )  SURFACE ( )  );
#9115 = CARTESIAN_POINT ( 'NONE',  ( 43.34962307344081012, 50.89948385550241028, 2.184720259617164650 ) ) ;
#9116 = ORIENTED_EDGE ( 'NONE', *, *, #3874, .F. ) ;
#9117 = ORIENTED_EDGE ( 'NONE', *, *, #12236, .F. ) ;
#9118 = CARTESIAN_POINT ( 'NONE',  ( 3.958491816111018746, 1.406739583089935186, 3.500000000000000000 ) ) ;
#9119 = VERTEX_POINT ( 'NONE', #8669 ) ;
#9120 = CARTESIAN_POINT ( 'NONE',  ( 6.371919382990606451, -1.972754410575515704, -5.108792907957607099 ) ) ;
#9121 = AXIS2_PLACEMENT_3D ( 'NONE', #5629, #3343, #3211 ) ;
#9122 = EDGE_CURVE ( 'NONE', #3301, #6976, #3528, .T. ) ;
#9123 = CARTESIAN_POINT ( 'NONE',  ( 18.00000000000000355, -20.00000000000000000, -20.00000000000000000 ) ) ;
#9124 = CARTESIAN_POINT ( 'NONE',  ( 46.49166364869456913, 58.30051614449765651, -4.867452303228181343 ) ) ;
#9125 = CARTESIAN_POINT ( 'NONE',  ( 4.000000000000000888, 0.8228435280416209752, -3.430609588141487976 ) ) ;
#9126 = CARTESIAN_POINT ( 'NONE',  ( 45.27934281921075410, 57.29948385550240175, -6.458785618021043895 ) ) ;
#9127 = CARTESIAN_POINT ( 'NONE',  ( 52.25172492374522903, 63.59948385550237759, -7.007379884777225953 ) ) ;
#9128 = CARTESIAN_POINT ( 'NONE',  ( -4.197393957002303999, -7.773935952363655451E-14, -3.503767560748929810 ) ) ;
#9129 = EDGE_CURVE ( 'NONE', #7204, #3958, #8234, .T. ) ;
#9130 = CARTESIAN_POINT ( 'NONE',  ( 47.37792948025162332, 51.39948385550241028, -7.992620115222770494 ) ) ;
#9131 = ORIENTED_EDGE ( 'NONE', *, *, #6453, .T. ) ;
#9132 = EDGE_LOOP ( 'NONE', ( #9101, #13225, #263, #9202 ) ) ;
#9133 = ORIENTED_EDGE ( 'NONE', *, *, #6993, .F. ) ;
#9134 = ORIENTED_EDGE ( 'NONE', *, *, #4660, .F. ) ;
#9135 = DIRECTION ( 'NONE',  ( 1.000000000000000000, 0.000000000000000000, 0.000000000000000000 ) ) ;
#9136 = CARTESIAN_POINT ( 'NONE',  ( -74.99999999999997158, -7.499999999999971578, -10.00000000000000000 ) ) ;
#9137 = SURFACE_SIDE_STYLE ('',( #6110 ) ) ;
#9138 = CYLINDRICAL_SURFACE ( 'NONE', #262, 12.49999999999999645 ) ;
#9139 = DIRECTION ( 'NONE',  ( 1.000000000000000000, 0.000000000000000000, 0.000000000000000000 ) ) ;
#9140 = CARTESIAN_POINT ( 'NONE',  ( 7.336184427528458230, 0.000000000000000000, 0.000000000000000000 ) ) ;
#9141 = CARTESIAN_POINT ( 'NONE',  ( 44.88205777487398507, 61.19948385550241454, -3.688883143319540814 ) ) ;
#9142 = CARTESIAN_POINT ( 'NONE',  ( 54.09612160359792199, 55.30051614449765651, 5.676469297603124353 ) ) ;
#9143 = EDGE_CURVE ( 'NONE', #8675, #10162, #13121, .T. ) ;
#9144 = CARTESIAN_POINT ( 'NONE',  ( 43.20883090819742023, 56.20051614449766220, -4.963592699178938972 ) ) ;
#9145 = EDGE_CURVE ( 'NONE', #8775, #3906, #11479, .T. ) ;
#9146 = SURFACE_STYLE_FILL_AREA ( #2635 ) ;
#9147 = FACE_OUTER_BOUND ( 'NONE', #12085, .T. ) ;
#9148 = CARTESIAN_POINT ( 'NONE',  ( 52.62207051974829852, 52.60051614449765367, -7.992620115222797139 ) ) ;
#9150 = VERTEX_POINT ( 'NONE', #1293 ) ;
#9149 = ORIENTED_EDGE ( 'NONE', *, *, #9814, .T. ) ;
#9151 = CARTESIAN_POINT ( 'NONE',  ( -1.393927851585477606, 4.043713361053528743, -3.526374918436835149 ) ) ;
#9152 = ORIENTED_EDGE ( 'NONE', *, *, #1798, .T. ) ;
#9153 = ORIENTED_EDGE ( 'NONE', *, *, #9413, .T. ) ;
#9154 = CARTESIAN_POINT ( 'NONE',  ( 1.000000000000000000, -14.00000000000000000, -9.000000000000001776 ) ) ;
#9155 = AXIS2_PLACEMENT_3D ( 'NONE', #7857, #776, #11230 ) ;
#9156 = CARTESIAN_POINT ( 'NONE',  ( -30.00000000000000000, -5.000000000000010658, 6.123233995736766282E-16 ) ) ;
#9157 = APPLICATION_PROTOCOL_DEFINITION ( 'draft international standard', 'automotive_design', 1998, #13418 ) ;
#9158 = CARTESIAN_POINT ( 'NONE',  ( 43.33558569842703179, 63.09948385550240602, -2.141517661632099223 ) ) ;
#9159 = CARTESIAN_POINT ( 'NONE',  ( 44.05948171654949874, 56.79948385550239465, 4.345558710429104465 ) ) ;
#9160 = VECTOR ( 'NONE', #5050, 1000.000000000000000 ) ;
#9161 = EDGE_CURVE ( 'NONE', #5207, #6478, #2631, .T. ) ;
#9162 = CARTESIAN_POINT ( 'NONE',  ( 0.3126073911696407026, -2.020725942163686728, 3.500000000000000444 ) ) ;
#9163 = AXIS2_PLACEMENT_3D ( 'NONE', #1633, #2610, #13116 ) ;
#9164 = DIRECTION ( 'NONE',  ( -1.000000000000000000, 0.000000000000000000, 0.000000000000000000 ) ) ;
#9165 = DIRECTION ( 'NONE',  ( 0.1305261922200524616, -0.9914448613738103822, 0.000000000000000000 ) ) ;
#9166 = CARTESIAN_POINT ( 'NONE',  ( 43.33558569842706021, 53.90051614449765793, 2.141517661632167169 ) ) ;
#9167 = CARTESIAN_POINT ( 'NONE',  ( 56.30877334542961421, 53.99948385550241170, -0.02388180880520959434 ) ) ;
#9168 = DIRECTION ( 'NONE',  ( 0.000000000000000000, 0.000000000000000000, -1.000000000000000000 ) ) ;
#9169 = ORIENTED_EDGE ( 'NONE', *, *, #6325, .T. ) ;
#9170 = AXIS2_PLACEMENT_3D ( 'NONE', #11598, #12488, #10347 ) ;
#9171 = VERTEX_POINT ( 'NONE', #9679 ) ;
#9172 = ORIENTED_EDGE ( 'NONE', *, *, #6407, .F. ) ;
#9173 = CARTESIAN_POINT ( 'NONE',  ( 4.093692494532771953, -2.021783646005774759, -3.501831996793842716 ) ) ;
#9174 = DIRECTION ( 'NONE',  ( -0.000000000000000000, -0.000000000000000000, -1.000000000000000000 ) ) ;
#9175 = AXIS2_PLACEMENT_3D ( 'NONE', #13298, #7098, #3842 ) ;
#9176 = CARTESIAN_POINT ( 'NONE',  ( 6.527192678185834929, -2.941622124011297412, 5.095038975455882913 ) ) ;
#9177 =( LENGTH_UNIT ( ) NAMED_UNIT ( * ) SI_UNIT ( .MILLI., .METRE. ) );
#9178 = CARTESIAN_POINT ( 'NONE',  ( 0.000000000000000000, -0.8865213383406694847, 1.535500000000001419 ) ) ;
#9179 = CARTESIAN_POINT ( 'NONE',  ( 55.11794222512599362, 46.80051614449766362, -3.688883143319583446 ) ) ;
#9180 = DIRECTION ( 'NONE',  ( -1.224646799147353207E-16, 0.000000000000000000, -1.000000000000000000 ) ) ;
#9181 = CARTESIAN_POINT ( 'NONE',  ( 45.90387839640214196, 58.69948385550240033, 5.676469297603166098 ) ) ;
#9182 = CARTESIAN_POINT ( 'NONE',  ( 47.74827507625478518, 52.59948385550239180, 7.007379884777227730 ) ) ;
#9183 = VERTEX_POINT ( 'NONE', #6649 ) ;
#9184 = CARTESIAN_POINT ( 'NONE',  ( 56.65037692655918988, 51.89948385550241028, -2.184720259617163762 ) ) ;
#9185 = ORIENTED_EDGE ( 'NONE', *, *, #2544, .F. ) ;
#9186 = ORIENTED_EDGE ( 'NONE', *, *, #10321, .F. ) ;
#9187 = CARTESIAN_POINT ( 'NONE',  ( 5.599999999999999645, -2.020725942163694722, -3.499999999999999556 ) ) ;
#9188 = ORIENTED_EDGE ( 'NONE', *, *, #5603, .F. ) ;
#9189 = CARTESIAN_POINT ( 'NONE',  ( -3.309651814758565180, -5.455921364805393026, -1.000000000000000000 ) ) ;
#9190 = CARTESIAN_POINT ( 'NONE',  ( 50.00000000000000000, 40.00000000000000000, -4.000000000000003553 ) ) ;
#9191 = CARTESIAN_POINT ( 'NONE',  ( 0.000000000000000000, 0.000000000000000000, 0.000000000000000000 ) ) ;
#9192 = AXIS2_PLACEMENT_3D ( 'NONE', #5232, #7088, #10535 ) ;
#9193 = CARTESIAN_POINT ( 'NONE',  ( 48.02776887271750184, 61.60051614449765367, 5.992620115222795363 ) ) ;
#9194 = CIRCLE ( 'NONE', #8091, 1.499999999999999334 ) ;
#9195 = CARTESIAN_POINT ( 'NONE',  ( -4.197393957002303999, -7.773935952363655451E-14, -3.503767560748929810 ) ) ;
#9196 = SHAPE_REPRESENTATION ( 'hex flange bolt small_iso_ISO 4162 - M8 x 45 x 22-N', ( #430 ), #7942 ) ;
#9197 = CARTESIAN_POINT ( 'NONE',  ( 43.18075615816989199, 59.19948385550240744, -4.924951120819313743 ) ) ;
#9198 = CARTESIAN_POINT ( 'NONE',  ( 49.97728705011488159, 61.49948385550240459, -7.000000000000000888 ) ) ;
#9199 = CARTESIAN_POINT ( 'NONE',  ( 0.4465819873851989974, -2.886751345948120218, 4.999999999999999112 ) ) ;
#9200 = CARTESIAN_POINT ( 'NONE',  ( 58.41169779390614281, 51.99948385550239749, -0.02388180880523160798 ) ) ;
#9201 = ORIENTED_EDGE ( 'NONE', *, *, #1991, .T. ) ;
#9202 = ORIENTED_EDGE ( 'NONE', *, *, #2185, .T. ) ;
#9203 = APPLICATION_CONTEXT ( 'automotive_design' ) ;
#9204 = VERTEX_POINT ( 'NONE', #12032 ) ;
#9205 = EDGE_CURVE ( 'NONE', #11896, #1915, #6866, .T. ) ;
#9206 = CARTESIAN_POINT ( 'NONE',  ( 2.449293598294706513E-15, -20.00000000000000000, -20.00000000000000000 ) ) ;
#9207 = CIRCLE ( 'NONE', #5199, 2.000000000000001332 ) ;
#9208 = CARTESIAN_POINT ( 'NONE',  ( -2.649999999999989697, 15.00000000000001599, -9.000000000000001776 ) ) ;
#9209 = DIRECTION ( 'NONE',  ( -0.000000000000000000, -0.000000000000000000, 1.000000000000000000 ) ) ;
#9210 = CARTESIAN_POINT ( 'NONE',  ( 1.999999999999998224, -3.464101615137772594, -3.142992957459239012 ) ) ;
#9211 = CARTESIAN_POINT ( 'NONE',  ( -59.84999999999998721, 32.50000000000001421, -15.00000000000000000 ) ) ;
#9212 = CARTESIAN_POINT ( 'NONE',  ( 55.08986747509847248, 61.79948385550240175, -3.727524721679197572 ) ) ;
#9213 = CARTESIAN_POINT ( 'NONE',  ( 49.97728705011495265, 55.50051614449766646, 7.000000000000000888 ) ) ;
#9214 = CARTESIAN_POINT ( 'NONE',  ( 56.81924384183006538, 60.80051614449766362, -4.924951120819380357 ) ) ;
#9215 = CARTESIAN_POINT ( 'NONE',  ( 5.000000000000003553, -20.00000000000000000, 15.00000000000000355 ) ) ;
#9216 = CARTESIAN_POINT ( 'NONE',  ( 42.39856655714564226, 50.10051614449766078, -2.493737253992044156 ) ) ;
#9218 = ORIENTED_EDGE ( 'NONE', *, *, #6637, .F. ) ;
#9217 = EDGE_LOOP ( 'NONE', ( #1845, #8188, #11482, #11145 ) ) ;
#9219 = ORIENTED_EDGE ( 'NONE', *, *, #7136, .F. ) ;
#9220 = ORIENTED_EDGE ( 'NONE', *, *, #1877, .T. ) ;
#9221 = VERTEX_POINT ( 'NONE', #1363 ) ;
#9222 = DIRECTION ( 'NONE',  ( -1.000000000000000000, 1.734723475976807094E-16, 0.000000000000000000 ) ) ;
#9223 = DIRECTION ( 'NONE',  ( 0.000000000000000000, -0.5000000000000011102, -0.8660254037844380415 ) ) ;
#9224 = APPLICATION_PROTOCOL_DEFINITION ( 'draft international standard', 'automotive_design', 1998, #1403 ) ;
#9225 = CARTESIAN_POINT ( 'NONE',  ( 43.34962307344081012, 64.89948385550239607, 2.184720259617164650 ) ) ;
#9226 = CARTESIAN_POINT ( 'NONE',  ( 54.09612160359786515, 61.69948385550240744, -5.676469297603166098 ) ) ;
#9227 = ADVANCED_FACE ( 'NONE', ( #8648, #2548 ), #3390, .F. ) ;
#9228 = DIRECTION ( 'NONE',  ( 1.000000000000000000, 0.000000000000000000, 0.000000000000000000 ) ) ;
#9229 = CARTESIAN_POINT ( 'NONE',  ( 3.129923130707922496, -23.63917314727666152, -9.999999999999994671 ) ) ;
#9230 = DIRECTION ( 'NONE',  ( 0.000000000000000000, 0.000000000000000000, -1.000000000000000000 ) ) ;
#9231 = CARTESIAN_POINT ( 'NONE',  ( 43.34962307344078880, 54.10051614449766788, -2.184720259617096705 ) ) ;
#9232 = CARTESIAN_POINT ( 'NONE',  ( 55.08986747509847248, 49.79948385550240175, -3.727524721679197572 ) ) ;
#9233 = CARTESIAN_POINT ( 'NONE',  ( 55.48859070151218020, 45.00000000000002132, -4.999999999999993783 ) ) ;
#9234 = EDGE_CURVE ( 'NONE', #1857, #2807, #4857, .T. ) ;
#9235 = ORIENTED_EDGE ( 'NONE', *, *, #6947, .T. ) ;
#9236 = ORIENTED_EDGE ( 'NONE', *, *, #9016, .F. ) ;
#9238 = ADVANCED_FACE ( 'NONE', ( #10914 ), #5677, .F. ) ;
#9237 = ORIENTED_EDGE ( 'NONE', *, *, #10558, .F. ) ;
#9239 = CARTESIAN_POINT ( 'NONE',  ( 2.449293598294706513E-15, -20.00000000000000000, 9.000000000000000000 ) ) ;
#9240 = EDGE_CURVE ( 'NONE', #3771, #4186, #7717, .T. ) ;
#9241 = AXIS2_PLACEMENT_3D ( 'NONE', #6853, #12376, #4717 ) ;
#9242 = CARTESIAN_POINT ( 'NONE',  ( 6.323279575527231522, 3.325091652218045368, -4.240772318537636920 ) ) ;
#9243 = DIRECTION ( 'NONE',  ( 1.000000000000000000, 0.000000000000000000, 0.000000000000000000 ) ) ;
#9244 = SURFACE_STYLE_FILL_AREA ( #7319 ) ;
#9245 = FACE_OUTER_BOUND ( 'NONE', #864, .T. ) ;
#9246 = CARTESIAN_POINT ( 'NONE',  ( 0.1404048886732821022, 4.699864953788070565, -3.686887068327037387 ) ) ;
#9247 = CARTESIAN_POINT ( 'NONE',  ( 55.69932041026405045, 47.10051614449766078, 1.875703265242156359 ) ) ;
#9248 = DIRECTION ( 'NONE',  ( 0.8660254037844374864, -0.5000000000000018874, 0.000000000000000000 ) ) ;
#9249 = CARTESIAN_POINT ( 'NONE',  ( 52.29715082351547295, 58.39948385550238896, 6.992620115222774047 ) ) ;
#9250 = CARTESIAN_POINT ( 'NONE',  ( 49.97728705011488159, 55.49948385550240459, -7.000000000000000888 ) ) ;
#9251 = AXIS2_PLACEMENT_3D ( 'NONE', #7925, #9859, #2591 ) ;
#9252 = ORIENTED_EDGE ( 'NONE', *, *, #13369, .F. ) ;
#9253 = CARTESIAN_POINT ( 'NONE',  ( 55.94051828345050836, 47.79948385550240886, -4.345558710429104465 ) ) ;
#9254 = CIRCLE ( 'NONE', #11236, 15.00000000000000000 ) ;
#9255 = EDGE_LOOP ( 'NONE', ( #9593, #4486, #8694, #2642 ) ) ;
#9256 = DIRECTION ( 'NONE',  ( -0.000000000000000000, 0.8660254037844383745, 0.5000000000000004441 ) ) ;
#9257 = VERTEX_POINT ( 'NONE', #12913 ) ;
#9258 = DIRECTION ( 'NONE',  ( -1.000000000000000000, 0.000000000000000000, 1.224646799147353207E-16 ) ) ;
#9259 = AXIS2_PLACEMENT_3D ( 'NONE', #7060, #3809, #10232 ) ;
#9260 = PLANE ( 'NONE',  #5418 ) ;
#9261 = PLANE ( 'NONE',  #5971 ) ;
#9262 = AXIS2_PLACEMENT_3D ( 'NONE', #12949, #7718, #2515 ) ;
#9263 = CARTESIAN_POINT ( 'NONE',  ( 55.08986747509849380, 63.20051614449766220, 3.727524721679155384 ) ) ;
#9264 = AXIS2_PLACEMENT_3D ( 'NONE', #4381, #11146, #1665 ) ;
#9265 = CARTESIAN_POINT ( 'NONE',  ( -4.211140560182196957, 2.431303136016537803, -3.745885042887433514 ) ) ;
#9266 = EDGE_CURVE ( 'NONE', #7290, #8677, #2765, .T. ) ;
#9267 = CARTESIAN_POINT ( 'NONE',  ( 50.02271294988513972, 60.49948385550240459, 8.000000000000001776 ) ) ;
#9268 = DIRECTION ( 'NONE',  ( 1.000000000000000000, 0.000000000000000000, 0.000000000000000000 ) ) ;
#9269 = STYLED_ITEM ( 'NONE', ( #853 ), #870 ) ;
#9270 = CARTESIAN_POINT ( 'NONE',  ( 42.39856655714566358, 50.89948385550240317, 2.493737253992119207 ) ) ;
#9271 = ORIENTED_EDGE ( 'NONE', *, *, #8475, .F. ) ;
#9272 = VERTEX_POINT ( 'NONE', #6516 ) ;
#9273 = EDGE_LOOP ( 'NONE', ( #9810, #9884, #12921, #7221 ) ) ;
#9274 = CARTESIAN_POINT ( 'NONE',  ( 5.599999999999998757, 0.000000000000000000, 0.000000000000000000 ) ) ;
#9275 = FILL_AREA_STYLE_COLOUR ( '', #10385 ) ;
#9276 = CARTESIAN_POINT ( 'NONE',  ( 0.000000000000000000, 0.000000000000000000, 0.000000000000000000 ) ) ;
#9277 = CARTESIAN_POINT ( 'NONE',  ( -31.74999999999995737, 0.000000000000000000, 2.000000000000000888 ) ) ;
#9278 = AXIS2_PLACEMENT_3D ( 'NONE', #13149, #2721, #7981 ) ;
#9279 = CARTESIAN_POINT ( 'NONE',  ( 1.274258131564866448, 3.883108878240963513, -3.220599429844046568 ) ) ;
#9280 = AXIS2_PLACEMENT_3D ( 'NONE', #2063, #12432, #3175 ) ;
#9281 = CARTESIAN_POINT ( 'NONE',  ( 51.97223112728249816, 44.60051614449766078, -5.992620115222793586 ) ) ;
#9282 = CARTESIAN_POINT ( 'NONE',  ( 57.36023556966787851, 51.00051614449765225, 0.02388180880515038476 ) ) ;
#9283 = CARTESIAN_POINT ( 'NONE',  ( 49.97728705011495265, 57.50051614449766646, 8.000000000000001776 ) ) ;
#9284 = FACE_OUTER_BOUND ( 'NONE', #12974, .T. ) ;
#9285 = CARTESIAN_POINT ( 'NONE',  ( 56.81924384183006538, 50.80051614449766362, -4.924951120819380357 ) ) ;
#9287 = ORIENTED_EDGE ( 'NONE', *, *, #12136, .T. ) ;
#9286 = ORIENTED_EDGE ( 'NONE', *, *, #8070, .F. ) ;
#9288 = VERTEX_POINT ( 'NONE', #8716 ) ;
#9289 = VERTEX_POINT ( 'NONE', #6777 ) ;
#9290 = LINE ( 'NONE', #13, #4483 ) ;
#9291 =( NAMED_UNIT ( * ) PLANE_ANGLE_UNIT ( ) SI_UNIT ( $, .RADIAN. ) );
#9292 = FACE_OUTER_BOUND ( 'NONE', #11794, .T. ) ;
#9293 = FACE_OUTER_BOUND ( 'NONE', #9759, .T. ) ;
#9294 = ITEM_DEFINED_TRANSFORMATION ( 'NONE', 'NONE', #8390,  #430 ) ;
#9295 = CARTESIAN_POINT ( 'NONE',  ( 55.69932041026404335, 45.89948385550240317, -1.875703265242203432 ) ) ;
#9296 = CARTESIAN_POINT ( 'NONE',  ( 55.94051828345050836, 61.79948385550240175, -4.345558710429103577 ) ) ;
#9297 = AXIS2_PLACEMENT_3D ( 'NONE', #6255, #12714, #888 ) ;
#9298 = CARTESIAN_POINT ( 'NONE',  ( 62.49999999999998579, 45.00000000000001421, -5.000000000000000000 ) ) ;
#9299 = DIRECTION ( 'NONE',  ( 0.000000000000000000, 1.000000000000000000, 0.000000000000000000 ) ) ;
#9300 = CARTESIAN_POINT ( 'NONE',  ( 8.500000000000000000, 2.886751345948123770, -5.000000000000000000 ) ) ;
#9301 = CARTESIAN_POINT ( 'NONE',  ( 54.09612160359792199, 51.30051614449766362, 5.676469297603124353 ) ) ;
#9302 = CARTESIAN_POINT ( 'NONE',  ( 55.11794222512601493, 54.19948385550241454, 3.688883143319541702 ) ) ;
#9303 = DIRECTION ( 'NONE',  ( 1.000000000000000000, 0.000000000000000000, 0.000000000000000000 ) ) ;
#9304 = EDGE_CURVE ( 'NONE', #720, #8082, #1496, .T. ) ;
#9305 = ORIENTED_EDGE ( 'NONE', *, *, #4410, .F. ) ;
#9306 = CARTESIAN_POINT ( 'NONE',  ( 1.498123826657866253, -34.92499999999999716, 9.000000000000000000 ) ) ;
#9307 = VERTEX_POINT ( 'NONE', #1851 ) ;
#9308 = ORIENTED_EDGE ( 'NONE', *, *, #103, .T. ) ;
#9309 = DIRECTION ( 'NONE',  ( 0.000000000000000000, 0.000000000000000000, 1.000000000000000000 ) ) ;
#9310 = VECTOR ( 'NONE', #6892, 1000.000000000000000 ) ;
#9311 = DIRECTION ( 'NONE',  ( -0.000000000000000000, -0.000000000000000000, -1.000000000000000000 ) ) ;
#9312 = CARTESIAN_POINT ( 'NONE',  ( 6.495567275915087535, -2.917443832164882345, 5.053160945538040849 ) ) ;
#9313 =( NAMED_UNIT ( * ) SI_UNIT ( $, .STERADIAN. ) SOLID_ANGLE_UNIT ( ) );
#9314 = ADVANCED_FACE ( 'NONE', ( #1782 ), #7944, .T. ) ;
#9315 = CARTESIAN_POINT ( 'NONE',  ( -0.6640947660597427138, 4.471078309994878985, -3.602146406945963442 ) ) ;
#9316 = CARTESIAN_POINT ( 'NONE',  ( 51.92680522751238925, 45.40051614449765793, 6.007379884777208190 ) ) ;
#9317 = EDGE_CURVE ( 'NONE', #3838, #5822, #3797, .T. ) ;
#9318 = LINE ( 'NONE', #4061, #7410 ) ;
#9319 = CARTESIAN_POINT ( 'NONE',  ( 50.02271294988512551, 64.49948385550240459, 7.000000000000000888 ) ) ;
#9320 = CARTESIAN_POINT ( 'NONE',  ( 45.90387839640214196, 50.69948385550240744, 5.676469297603166098 ) ) ;
#9321 = AXIS2_PLACEMENT_3D ( 'NONE', #1445, #2422, #5691 ) ;
#9322 = ADVANCED_FACE ( 'NONE', ( #8019 ), #2614, .T. ) ;
#9323 = AXIS2_PLACEMENT_3D ( 'NONE', #2065, #6863, #12114 ) ;
#9324 = VECTOR ( 'NONE', #2376, 1000.000000000000000 ) ;
#9325 = ORIENTED_EDGE ( 'NONE', *, *, #2665, .F. ) ;
#9326 = CARTESIAN_POINT ( 'NONE',  ( 55.96859303347804371, 48.19948385550240033, 4.306917132069425946 ) ) ;
#9327 = ORIENTED_EDGE ( 'NONE', *, *, #2720, .F. ) ;
#9328 = PLANE ( 'NONE',  #13421 ) ;
#9329 = ORIENTED_EDGE ( 'NONE', *, *, #3984, .F. ) ;
#9330 = CARTESIAN_POINT ( 'NONE',  ( 4.132952817037859994, 2.031684012687258623, 3.518979934899746809 ) ) ;
#9331 = CIRCLE ( 'NONE', #13283, 5.000000000000000000 ) ;
#9332 = DIRECTION ( 'NONE',  ( 1.000000000000000000, -1.734723475976807341E-16, -0.000000000000000000 ) ) ;
#9333 = CIRCLE ( 'NONE', #2693, 2.649999999999988365 ) ;
#9334 = DIRECTION ( 'NONE',  ( 0.1305261922200524616, 0.9914448613738103822, -0.000000000000000000 ) ) ;
#9335 = CARTESIAN_POINT ( 'NONE',  ( 54.13287192849671214, 44.70051614449766220, -5.649768623646139964 ) ) ;
#9336 = CARTESIAN_POINT ( 'NONE',  ( -74.99999999999997158, 40.00000000000001421, 10.00000000000000000 ) ) ;
#9337 = CARTESIAN_POINT ( 'NONE',  ( 58.41169779390614281, 59.99948385550241170, -0.02388180880523160798 ) ) ;
#9338 = DIRECTION ( 'NONE',  ( -1.000000000000000000, -0.000000000000000000, -0.000000000000000000 ) ) ;
#9339 = CARTESIAN_POINT ( 'NONE',  ( 52.62207051974839089, 48.39948385550240317, 7.992620115222770494 ) ) ;
#9340 = VERTEX_POINT ( 'NONE', #11117 ) ;
#9341 = ORIENTED_EDGE ( 'NONE', *, *, #7707, .T. ) ;
#9342 = CIRCLE ( 'NONE', #6909, 0.7500000000000000000 ) ;
#9343 = ORIENTED_EDGE ( 'NONE', *, *, #5953, .T. ) ;
#9344 = FACE_OUTER_BOUND ( 'NONE', #7521, .T. ) ;
#9345 = CIRCLE ( 'NONE', #3380, 4.800000000000000711 ) ;
#9346 = FILL_AREA_STYLE ('',( #1273 ) ) ;
#9347 = CARTESIAN_POINT ( 'NONE',  ( 2.449293598294706513E-15, -20.00000000000000000, -10.00000000000000000 ) ) ;
#9348 = CARTESIAN_POINT ( 'NONE',  ( 6.445127866599367650, -5.657054305385780246, -0.4229901806197432501 ) ) ;
#9349 = CARTESIAN_POINT ( 'NONE',  ( 0.5449313310647804220, 4.304185902836899835, -3.316620875263383894 ) ) ;
#9350 = CARTESIAN_POINT ( 'NONE',  ( 55.71335778527780747, 62.09948385550240602, 1.832500667257165983 ) ) ;
#9351 = CARTESIAN_POINT ( 'NONE',  ( 42.63976443033212149, 58.00051614449765225, -0.02388180880514948964 ) ) ;
#9352 = CARTESIAN_POINT ( 'NONE',  ( 45.27934281921082516, 61.70051614449766220, 6.458785618021089192 ) ) ;
#9353 = ADVANCED_FACE ( 'NONE', ( #6027 ), #11048, .F. ) ;
#9354 = VECTOR ( 'NONE', #9338, 1000.000000000000000 ) ;
#9355 = CARTESIAN_POINT ( 'NONE',  ( -7.500000000000013323, -7.009618943233427935, 9.000000000000000000 ) ) ;
#9356 = CARTESIAN_POINT ( 'NONE',  ( 56.79116909180259398, 49.20051614449766220, 4.963592699178938972 ) ) ;
#9358 = ORIENTED_EDGE ( 'NONE', *, *, #12029, .F. ) ;
#9357 = ORIENTED_EDGE ( 'NONE', *, *, #13352, .T. ) ;
#9359 = ORIENTED_EDGE ( 'NONE', *, *, #590, .T. ) ;
#9360 = ORIENTED_EDGE ( 'NONE', *, *, #10318, .F. ) ;
#9361 =( BOUNDED_SURFACE ( )  B_SPLINE_SURFACE ( 3, 2, ( 
 ( #3020, #9385, #11239, #2812, #6080, #13582, #1761, #6223, #5177, #10343, #4964, #13370, #1832, #7320, #8139, #12345, #2879, #7100, #11310, #10276, #786, #3982, #8210, #12413, #2372, #7509, #2308, #7646, #5507, #9646, #6355, #6547, #238, #11784, #11717, #4387, #10748, #1126, #3225, #10617, #1253, #5377, #9714, #4458, #2238, #10547, #6607, #11594, #39, #10808, #12811, #2106, #11652, #1198, #8684, #1058, #3288, #1325, #4264, #5308, #12877, #9583, #11852, #9513, #8482, #12684, #5572, #7383, #107, #4326, #7447, #3424, #10685, #6484, #13645, #4193, #8613, #5447, #170, #8417, #12743, #12622, #3157, #3355, #2172, #8548, #6417, #7577, #11152, #4665, #8816, #368, #5781, #2581, #3691, #9781, #494, #10043, #11083, #1391, #6806, #9976, #2722, #300, #7914, #13015, #6874, #11012, #12125, #9910, #12943, #5709, #7783, #4735, #13211, #3628, #2650, #8951, #1599, #4801, #3558, #6679, #11994, #13150, #3759, #7850, #5845, #556, #9013, #7982, #2511, #10877, #5643, #10948, #8749, #6744, #12194, #9848, #1533, #6944, #3489, #4528, #1463, #1670, #7713, #11918, #2440, #12061, #4596, #429, #8887, #13083, #5987, #8334, #7157, #11366, #12535, #1887, #11508, #13420, #906, #9087, #3064, #3963, #8262, #13563, #11429, #6130, #12261, #12465, #6198, #4040, #8192, #10326, #3001, #7084, #9158, #2860, #7229, #11293, #1954, #10395, #12396, #2794, #7300, #3830, #10189, #5912, #5087, #8054, #3894, #829, #5160, #7011, #9225, #10111, #697, #11219, #9365, #1816, #4110 ),
 ( #4947, #1742, #621, #13353, #9295, #2934, #13488, #8122, #4874, #12325, #13286, #6062, #10256, #767, #5019, #2153, #1178, #2287, #4310, #3134, #976, #7492, #12797, #6400, #1107, #7431, #4173, #11637, #9565, #4372, #5358, #10530, #11575, #8396, #2090, #10600, #8461, #8529, #9630, #86, #5227, #12729, #13626, #8593, #6531, #12604, #155, #9493, #7367, #222, #6271, #11698, #8667, #10668, #3271, #2221, #17, #10729, #6335, #6465, #1039, #3206, #7562, #5430, #3338, #4441, #11770, #1240, #5488, #9696, #12863, #3406, #7628, #5290, #2024, #4241, #10461, #9429, #12665, #9961, #412, #1309, #5693, #6592, #13196, #4650, #1517, #3678, #13069, #6794, #287, #479, #5763, #3614, #7765, #8999, #3745, #11832, #3474, #4720, #11902, #6662, #12927, #5832, #10863, #7835, #9893, #8868, #5624, #544, #4580, #11062, #8737, #2355, #10993, #8938, #11978, #13137, #12111, #12047, #7693, #10789, #2565, #7901, #2497, #10932, #3541, #4510, #6729, #2632, #6858, #1447, #1378, #2424, #8796, #1584, #12998, #4788, #10029, #5554, #9834, #9766, #353, #10174, #13471, #4999, #890, #13334, #10378, #605, #8034, #13267, #5142, #13402, #11204, #7210, #2988, #9141, #8247, #4858, #6999, #10096, #3881, #9212, #7067, #9073, #9350, #3948, #12311, #13545, #1797, #11135, #1655, #5972, #7140, #12246, #7966, #8177, #12381, #12178, #2915, #2703, #6045, #11415, #5899, #6928, #10237, #10308, #1935, #4021, #11348, #3815, #815, #12446, #6114, #750, #1870, #5067, #8107, #1725, #4929 ),
 ( #2778, #9281, #6182, #676, #2844, #11278, #5474, #6384, #7477, #9615, #5341, #12716, #6257, #6447, #11683, #9547, #1, #1228, #9678, #4095, #9416, #2204, #4156, #12587, #5214, #11751, #3118, #72, #2138, #11624, #11563, #6515, #10513, #3323, #956, #8317, #3257, #10650, #4224, #1164, #4358, #10581, #13614, #3049, #4292, #5410, #8445, #3188, #9476, #10448, #12651, #1089, #138, #7418, #7351, #8380, #1026, #8577, #5275, #10715, #12779, #7541, #2073, #2269, #12517, #6322, #7279, #8516, #11491, #2009, #2613, #6576, #269, #5537, #6839, #5676, #3457, #13120, #8922, #1361, #464, #10775, #12912, #2338, #9816, #1428, #12980, #1292, #11046, #9876, #4562, #12030, #7749, #4633, #6776, #5607, #7677, #10843, #10977, #336, #2546, #5743, #11956, #9749, #1566, #11815, #4491, #5814, #13049, #8715, #11885, #398, #4703, #2406, #3524, #203, #6647, #8781, #9943, #2478, #12091, #6712, #10913, #8851, #4424, #7611, #3594, #7816, #1495, #3660, #7886, #8647, #12845, #3389, #731, #11260, #13316, #13455, #9124, #4770, #10292, #8090, #7123, #10152, #13181, #8982, #11400, #4911, #9051, #586, #6026, #2827, #3930, #10010, #4984, #802, #11327, #1636, #7049, #10223, #2969, #2686, #10079, #657, #2760, #1781, #8160, #3864, #3721, #5952, #8017, #9193, #4004, #12296, #2898, #13388, #12365, #5052, #3796, #6911, #11116, #11186, #7948, #12226, #1850, #5880, #6100, #9263, #12161, #4838, #6981, #8231, #1921, #12431, #7196, #527, #13248, #1706, #4143, #5325, #6241 ),
 ( #12789, #1150, #9335, #8563, #4211, #8501, #126, #11666, #2125, #12501, #12703, #6435, #3243, #8364, #2191, #3174, #12765, #11548, #3308, #3034, #10434, #11470, #7530, #11611, #9403, #5398, #9603, #7336, #10635, #7261, #5196, #8300, #2062, #7401, #5262, #1994, #11738, #6369, #10499, #6164, #4076, #7465, #4347, #946, #60, #13598, #12572, #10364, #873, #10563, #5125, #1073, #9461, #9532, #3104, #13528, #6306, #8433, #1010, #12640, #4280, #10896, #10829, #4687, #3580, #1415, #6699, #2460, #7666, #11870, #9929, #5523, #5594, #9737, #5661, #2391, #8908, #384, #4549, #5464, #9803, #10705, #3647, #8769, #9865, #7803, #3510, #4618, #4412, #8837, #13035, #7735, #6632, #13103, #7869, #2256, #7599, #12014, #2326, #10764, #3376, #449, #1277, #11940, #323, #12964, #254, #6504, #8701, #1480, #12833, #1217, #2530, #6762, #1347, #10964, #5729, #9667, #11805, #188, #8631, #6564, #4479, #12900, #3444, #514, #8002, #5932, #911, #1690, #6897, #7931, #9034, #7231, #13233, #978, #3068, #2028, #12146, #8336, #5869, #8968, #10463, #2597, #3847, #5230, #11432, #10133, #13303, #10061, #7303, #13166, #641, #9996, #3778, #4112, #1957, #6968, #9431, #13566, #6201, #3003, #12467, #12213, #2742, #6274, #1621, #4892, #574, #10397, #11171, #13628, #5162, #9108, #1550, #8265, #6824, #4176, #9367, #12537, #11510, #12078, #11031, #4755, #5799, #3708, #2669, #11103, #4820, #289, #8400, #20, #2291, #8463, #3209, #9496, #2357, #7433, #158, #6468, #2223 ),
 ( #10671, #5490, #8532, #11578, #3139, #9768, #3273, #11639, #12667, #4374, #1180, #6533, #12606, #12799, #8670, #9699, #4245, #5432, #8595, #1311, #1041, #2156, #12731, #1109, #9632, #10731, #7495, #2092, #4312, #6403, #3340, #11834, #7564, #1242, #11772, #224, #3409, #10602, #5293, #5362, #9567, #7369, #88, #4443, #11700, #12865, #7632, #6337, #10533, #6594, #10792, #5556, #12113, #11064, #12049, #7695, #11904, #2499, #3680, #4583, #9001, #1380, #2634, #11980, #5627, #2705, #8739, #9963, #11138, #13139, #7838, #5765, #6731, #13198, #9836, #2567, #2426, #5695, #10032, #7903, #13070, #6930, #5834, #6861, #8941, #4722, #9896, #414, #12181, #7767, #6796, #10934, #1586, #4652, #1657, #546, #10995, #6664, #1520, #12930, #5901, #481, #4790, #3747, #7968, #10098, #10865, #4513, #3476, #355, #8871, #8798, #13000, #3543, #1450, #3616, #678, #9144, #1727, #8319, #13338, #6116, #12383, #8179, #8109, #3051, #7069, #13548, #11206, #4860, #9283, #4023, #753, #13473, #892, #2917, #5974, #13269, #10311, #11417, #5002, #13404, #6047, #2780, #10240, #7143, #2990, #3950, #3883, #10176, #11280, #8249, #1800, #7282, #5144, #4098, #4931, #10380, #7213, #2846, #6184, #11351, #11493, #9214, #2011, #7001, #12313, #1873, #6259, #817, #5069, #12520, #9352, #12450, #607, #1938, #9075, #3818, #8037, #12249, #9550, #3120, #3392, #2206, #1092, #7614, #8382, #12781, #5413, #12590, #3325, #140, #11686, #6386, #11818, #2340, #10450, #2076, #4360, #10516, #5277 ),
 ( #6450, #74, #206, #4294, #5217, #10717, #8518, #7543, #10584, #13616, #9419, #959, #5343, #9479, #1028, #10652, #3259, #8579, #4159, #1166, #1230, #11754, #6324, #7480, #9617, #7353, #11565, #3, #12718, #3191, #2272, #6518, #5476, #4227, #9680, #8447, #4427, #8649, #12847, #12653, #7420, #11626, #2141, #338, #3460, #7679, #7752, #5540, #8783, #466, #11887, #12033, #12093, #9751, #1295, #12982, #2615, #7951, #4705, #13123, #400, #271, #4493, #4564, #5746, #6650, #8985, #7818, #2549, #13183, #6778, #12164, #4635, #1568, #8719, #3723, #8854, #8924, #530, #6842, #10979, #12914, #3664, #11049, #7888, #13051, #1497, #5817, #11958, #9819, #3527, #10012, #2480, #4772, #6578, #3596, #2408, #10777, #10845, #1364, #5609, #9946, #6715, #10916, #1430, #5678, #9878, #6028, #4078, #11188, #3798, #10367, #1709, #8162, #733, #10224, #10154, #5127, #9126, #1923, #13251, #6914, #11329, #6102, #2830, #1852, #2971, #4987, #8020, #1639, #12367, #13457, #7052, #1783, #8093, #4840, #12298, #9197, #5055, #13390, #5955, #12228, #13318, #10295, #3866, #9337, #7199, #6167, #2762, #12433, #9267, #4913, #8235, #3934, #13531, #11263, #8302, #9053, #6983, #659, #2688, #2901, #7125, #875, #11403, #804, #11118, #4007, #5883, #10082, #589, #62, #11613, #5200, #5466, #4282, #3176, #9669, #10436, #1152, #3311, #9405, #6437, #6310, #13601, #10707, #3036, #8504, #191, #7468, #2128, #12705, #10502, #7532, #4145, #10566, #948, #7950, #4349, #11670, #7404 ),
 ( #9606, #4213, #10640, #8565, #6372, #8368, #1219, #12574, #3107, #4415, #2193, #7338, #1014, #3245, #12769, #11550, #1075, #12503, #2064, #5264, #11741, #8436, #7265, #9464, #12642, #5329, #11475, #6243, #9535, #5400, #128, #2259, #6506, #1996, #518, #8634, #257, #2532, #8704, #3446, #9740, #2601, #7669, #386, #6702, #5803, #12837, #6635, #12081, #7738, #3378, #8911, #10898, #5732, #8771, #11807, #7601, #9999, #3513, #11872, #12902, #4622, #1417, #6764, #2329, #13037, #13106, #9932, #4481, #5664, #8839, #1553, #1280, #2394, #12967, #1352, #9867, #10967, #11942, #6567, #4551, #10831, #3583, #6828, #2464, #1482, #7805, #451, #3650, #5596, #5525, #9805, #326, #10766, #12017, #4691, #7872, #11034, #10281, #7935, #13169, #6972, #791, #6153, #12353, #11315, #12284, #12149, #2672, #2747, #3918, #4823, #7182, #6008, #10210, #11389, #718, #10348, #2816, #13441, #6901, #1910, #7035, #7106, #12419, #5040, #4970, #11106, #1837, #9249, #2884, #11245, #9181, #6087, #5936, #8006, #1695, #3990, #10138, #8215, #2957, #1766, #1625, #4758, #5872, #9038, #8971, #8144, #10065, #11175, #13375, #3711, #577, #8078, #13236, #3782, #12217, #645, #4896, #9112, #13307, #3852, #7249, #933, #5249, #7325, #7387, #8487, #999, #4062, #10487, #12560, #10551, #4331, #8423, #7452, #1062, #12690, #9589, #8355, #11455, #1980, #2047, #13512, #3092, #3230, #6228, #6359, #6424, #8288, #9319, #11535, #10622, #2243, #11656, #2176, #12626, #12489, #3024, #6295, #44 ) ),
 .UNSPECIFIED., .T., .F., .F. ) 
 B_SPLINE_SURFACE_WITH_KNOTS ( ( 4, 3, 4 ),
 ( 3, 2, 2, 2, 2, 2, 2, 2, 2, 2, 2, 2, 2, 2, 2, 2, 2, 2, 2, 2, 2, 2, 2, 2, 2, 2, 2, 2, 2, 2, 2, 2, 2, 2, 2, 2, 2, 2, 2, 2, 2, 2, 2, 2, 2, 2, 2, 2, 2, 2, 2, 2, 2, 2, 2, 2, 2, 2, 2, 2, 2, 2, 2, 2, 2, 2, 2, 2, 2, 2, 2, 2, 2, 2, 2, 2, 2, 2, 2, 2, 2, 2, 2, 2, 2, 2, 2, 2, 2, 2, 2, 2, 2, 2, 2, 2, 2, 2, 2, 2, 3 ),
 ( 0.000000000000000000, 0.5000000000000000000, 1.000000000000000000 ),
 ( 0.000000000000000000, 0.01000000000000000021, 0.02000000000000000042, 0.02999999999999999889, 0.04000000000000000083, 0.05000000000000000278, 0.05999999999999999778, 0.07000000000000000666, 0.08000000000000000167, 0.08999999999999999667, 0.1000000000000000056, 0.1100000000000000006, 0.1199999999999999956, 0.1300000000000000044, 0.1400000000000000133, 0.1499999999999999944, 0.1600000000000000033, 0.1700000000000000122, 0.1799999999999999933, 0.1900000000000000022, 0.2000000000000000111, 0.2099999999999999922, 0.2200000000000000011, 0.2300000000000000100, 0.2399999999999999911, 0.2500000000000000000, 0.2600000000000000089, 0.2700000000000000178, 0.2800000000000000266, 0.2899999999999999800, 0.2999999999999999889, 0.3099999999999999978, 0.3200000000000000067, 0.3300000000000000155, 0.3400000000000000244, 0.3499999999999999778, 0.3599999999999999867, 0.3699999999999999956, 0.3800000000000000044, 0.3900000000000000133, 0.4000000000000000222, 0.4099999999999999756, 0.4199999999999999845, 0.4299999999999999933, 0.4400000000000000022, 0.4500000000000000111, 0.4600000000000000200, 0.4699999999999999734, 0.4799999999999999822, 0.4899999999999999911, 0.5000000000000000000, 0.5100000000000000089, 0.5200000000000000178, 0.5300000000000000266, 0.5400000000000000355, 0.5500000000000000444, 0.5600000000000000533, 0.5699999999999999512, 0.5799999999999999600, 0.5899999999999999689, 0.5999999999999999778, 0.6099999999999999867, 0.6199999999999999956, 0.6300000000000000044, 0.6400000000000000133, 0.6500000000000000222, 0.6600000000000000311, 0.6700000000000000400, 0.6800000000000000488, 0.6899999999999999467, 0.6999999999999999556, 0.7099999999999999645, 0.7199999999999999734, 0.7299999999999999822, 0.7399999999999999911, 0.7500000000000000000, 0.7600000000000000089, 0.7700000000000000178, 0.7800000000000000266, 0.7900000000000000355, 0.8000000000000000444, 0.8100000000000000533, 0.8199999999999999512, 0.8299999999999999600, 0.8399999999999999689, 0.8499999999999999778, 0.8599999999999999867, 0.8699999999999999956, 0.8800000000000000044, 0.8900000000000000133, 0.9000000000000000222, 0.9100000000000000311, 0.9200000000000000400, 0.9300000000000000488, 0.9399999999999999467, 0.9499999999999999556, 0.9599999999999999645, 0.9699999999999999734, 0.9799999999999999822, 0.9899999999999999911, 1.000000000000000000 ),
 .UNSPECIFIED. ) 
 GEOMETRIC_REPRESENTATION_ITEM ( )  RATIONAL_B_SPLINE_SURFACE ( (
 ( 1.000000000000000000, 0.9510565162951535312, 1.000000000000000000, 0.9510565162951535312, 1.000000000000000000, 0.9510565162951535312, 1.000000000000000000, 0.9510565162951535312, 1.000000000000000000, 0.9510565162951535312, 1.000000000000000000, 0.9510565162951535312, 1.000000000000000000, 0.9510565162951535312, 1.000000000000000000, 0.9510565162951535312, 1.000000000000000000, 0.9510565162951535312, 1.000000000000000000, 0.9510565162951535312, 1.000000000000000000, 0.9510565162951535312, 1.000000000000000000, 0.9510565162951535312, 1.000000000000000000, 0.9510565162951535312, 1.000000000000000000, 0.9510565162951535312, 1.000000000000000000, 0.9510565162951535312, 1.000000000000000000, 0.9510565162951535312, 1.000000000000000000, 0.9510565162951535312, 1.000000000000000000, 0.9510565162951535312, 1.000000000000000000, 0.9510565162951535312, 1.000000000000000000, 0.9510565162951535312, 1.000000000000000000, 0.9510565162951535312, 1.000000000000000000, 0.9510565162951535312, 1.000000000000000000, 0.9510565162951535312, 1.000000000000000000, 0.9510565162951535312, 1.000000000000000000, 0.9510565162951535312, 1.000000000000000000, 0.9510565162951535312, 1.000000000000000000, 0.9510565162951535312, 1.000000000000000000, 0.9510565162951535312, 1.000000000000000000, 0.9510565162951535312, 1.000000000000000000, 0.9510565162951535312, 1.000000000000000000, 0.9510565162951535312, 1.000000000000000000, 0.9510565162951535312, 1.000000000000000000, 0.9510565162951535312, 1.000000000000000000, 0.9510565162951535312, 1.000000000000000000, 0.9510565162951535312, 1.000000000000000000, 0.9510565162951535312, 1.000000000000000000, 0.9510565162951535312, 1.000000000000000000, 0.9510565162951535312, 1.000000000000000000, 0.9510565162951535312, 1.000000000000000000, 0.9510565162951535312, 1.000000000000000000, 0.9510565162951535312, 1.000000000000000000, 0.9510565162951535312, 1.000000000000000000, 0.9510565162951535312, 1.000000000000000000, 0.9510565162951535312, 1.000000000000000000, 0.9510565162951535312, 1.000000000000000000, 0.9510565162951535312, 1.000000000000000000, 0.9510565162951535312, 1.000000000000000000, 0.9510565162951535312, 1.000000000000000000, 0.9510565162951535312, 1.000000000000000000, 0.9510565162951535312, 1.000000000000000000, 0.9510565162951535312, 1.000000000000000000, 0.9510565162951535312, 1.000000000000000000, 0.9510565162951535312, 1.000000000000000000, 0.9510565162951535312, 1.000000000000000000, 0.9510565162951535312, 1.000000000000000000, 0.9510565162951535312, 1.000000000000000000, 0.9510565162951535312, 1.000000000000000000, 0.9510565162951535312, 1.000000000000000000, 0.9510565162951535312, 1.000000000000000000, 0.9510565162951535312, 1.000000000000000000, 0.9510565162951535312, 1.000000000000000000, 0.9510565162951535312, 1.000000000000000000, 0.9510565162951535312, 1.000000000000000000, 0.9510565162951535312, 1.000000000000000000, 0.9510565162951535312, 1.000000000000000000, 0.9510565162951535312, 1.000000000000000000, 0.9510565162951535312, 1.000000000000000000, 0.9510565162951535312, 1.000000000000000000, 0.9510565162951535312, 1.000000000000000000, 0.9510565162951535312, 1.000000000000000000, 0.9510565162951535312, 1.000000000000000000, 0.9510565162951535312, 1.000000000000000000, 0.9510565162951535312, 1.000000000000000000, 0.9510565162951535312, 1.000000000000000000, 0.9510565162951535312, 1.000000000000000000, 0.9510565162951535312, 1.000000000000000000, 0.9510565162951535312, 1.000000000000000000, 0.9510565162951535312, 1.000000000000000000, 0.9510565162951535312, 1.000000000000000000, 0.9510565162951535312, 1.000000000000000000, 0.9510565162951535312, 1.000000000000000000, 0.9510565162951535312, 1.000000000000000000, 0.9510565162951535312, 1.000000000000000000, 0.9510565162951535312, 1.000000000000000000, 0.9510565162951535312, 1.000000000000000000, 0.9510565162951535312, 1.000000000000000000, 0.9510565162951535312, 1.000000000000000000, 0.9510565162951535312, 1.000000000000000000, 0.9510565162951535312, 1.000000000000000000, 0.9510565162951535312, 1.000000000000000000, 0.9510565162951535312, 1.000000000000000000, 0.9510565162951535312, 1.000000000000000000, 0.9510565162951535312, 1.000000000000000000, 0.9510565162951535312, 1.000000000000000000, 0.9510565162951535312, 1.000000000000000000, 0.9510565162951535312, 1.000000000000000000, 0.9510565162951535312, 1.000000000000000000, 0.9510565162951535312, 1.000000000000000000, 0.9510565162951535312, 1.000000000000000000, 0.9510565162951535312, 1.000000000000000000),
 ( 0.3333333333333333703, 0.3170188387650512141, 0.3333333333333333703, 0.3170188387650512141, 0.3333333333333333703, 0.3170188387650512141, 0.3333333333333333703, 0.3170188387650512141, 0.3333333333333333703, 0.3170188387650512141, 0.3333333333333333703, 0.3170188387650512141, 0.3333333333333333703, 0.3170188387650512141, 0.3333333333333333703, 0.3170188387650512141, 0.3333333333333333703, 0.3170188387650512141, 0.3333333333333333703, 0.3170188387650512141, 0.3333333333333333703, 0.3170188387650512141, 0.3333333333333333703, 0.3170188387650512141, 0.3333333333333333703, 0.3170188387650512141, 0.3333333333333333703, 0.3170188387650512141, 0.3333333333333333703, 0.3170188387650512141, 0.3333333333333333703, 0.3170188387650512141, 0.3333333333333333703, 0.3170188387650512141, 0.3333333333333333703, 0.3170188387650512141, 0.3333333333333333703, 0.3170188387650512141, 0.3333333333333333703, 0.3170188387650512141, 0.3333333333333333703, 0.3170188387650512141, 0.3333333333333333703, 0.3170188387650512141, 0.3333333333333333703, 0.3170188387650512141, 0.3333333333333333703, 0.3170188387650512141, 0.3333333333333333703, 0.3170188387650512141, 0.3333333333333333703, 0.3170188387650512141, 0.3333333333333333703, 0.3170188387650512141, 0.3333333333333333703, 0.3170188387650512141, 0.3333333333333333703, 0.3170188387650512141, 0.3333333333333333703, 0.3170188387650512141, 0.3333333333333333703, 0.3170188387650512141, 0.3333333333333333703, 0.3170188387650512141, 0.3333333333333333703, 0.3170188387650512141, 0.3333333333333333703, 0.3170188387650512141, 0.3333333333333333703, 0.3170188387650512141, 0.3333333333333333703, 0.3170188387650512141, 0.3333333333333333703, 0.3170188387650512141, 0.3333333333333333703, 0.3170188387650512141, 0.3333333333333333703, 0.3170188387650512141, 0.3333333333333333703, 0.3170188387650512141, 0.3333333333333333703, 0.3170188387650512141, 0.3333333333333333703, 0.3170188387650512141, 0.3333333333333333703, 0.3170188387650512141, 0.3333333333333333703, 0.3170188387650512141, 0.3333333333333333703, 0.3170188387650512141, 0.3333333333333333703, 0.3170188387650512141, 0.3333333333333333703, 0.3170188387650512141, 0.3333333333333333703, 0.3170188387650512141, 0.3333333333333333703, 0.3170188387650512141, 0.3333333333333333703, 0.3170188387650512141, 0.3333333333333333703, 0.3170188387650512141, 0.3333333333333333703, 0.3170188387650512141, 0.3333333333333333703, 0.3170188387650512141, 0.3333333333333333703, 0.3170188387650512141, 0.3333333333333333703, 0.3170188387650512141, 0.3333333333333333703, 0.3170188387650512141, 0.3333333333333333703, 0.3170188387650512141, 0.3333333333333333703, 0.3170188387650512141, 0.3333333333333333703, 0.3170188387650512141, 0.3333333333333333703, 0.3170188387650512141, 0.3333333333333333703, 0.3170188387650512141, 0.3333333333333333703, 0.3170188387650512141, 0.3333333333333333703, 0.3170188387650512141, 0.3333333333333333703, 0.3170188387650512141, 0.3333333333333333703, 0.3170188387650512141, 0.3333333333333333703, 0.3170188387650512141, 0.3333333333333333703, 0.3170188387650512141, 0.3333333333333333703, 0.3170188387650512141, 0.3333333333333333703, 0.3170188387650512141, 0.3333333333333333703, 0.3170188387650512141, 0.3333333333333333703, 0.3170188387650512141, 0.3333333333333333703, 0.3170188387650512141, 0.3333333333333333703, 0.3170188387650512141, 0.3333333333333333703, 0.3170188387650512141, 0.3333333333333333703, 0.3170188387650512141, 0.3333333333333333703, 0.3170188387650512141, 0.3333333333333333703, 0.3170188387650512141, 0.3333333333333333703, 0.3170188387650512141, 0.3333333333333333703, 0.3170188387650512141, 0.3333333333333333703, 0.3170188387650512141, 0.3333333333333333703, 0.3170188387650512141, 0.3333333333333333703, 0.3170188387650512141, 0.3333333333333333703, 0.3170188387650512141, 0.3333333333333333703, 0.3170188387650512141, 0.3333333333333333703, 0.3170188387650512141, 0.3333333333333333703, 0.3170188387650512141, 0.3333333333333333703, 0.3170188387650512141, 0.3333333333333333703, 0.3170188387650512141, 0.3333333333333333703, 0.3170188387650512141, 0.3333333333333333703, 0.3170188387650512141, 0.3333333333333333703, 0.3170188387650512141, 0.3333333333333333703, 0.3170188387650512141, 0.3333333333333333703, 0.3170188387650512141, 0.3333333333333333703, 0.3170188387650512141, 0.3333333333333333703, 0.3170188387650512141, 0.3333333333333333703, 0.3170188387650512141, 0.3333333333333333703, 0.3170188387650512141, 0.3333333333333333703, 0.3170188387650512141, 0.3333333333333333703, 0.3170188387650512141, 0.3333333333333333703, 0.3170188387650512141, 0.3333333333333333703),
 ( 0.3333333333333333703, 0.3170188387650512141, 0.3333333333333333703, 0.3170188387650512141, 0.3333333333333333703, 0.3170188387650512141, 0.3333333333333333703, 0.3170188387650512141, 0.3333333333333333703, 0.3170188387650512141, 0.3333333333333333703, 0.3170188387650512141, 0.3333333333333333703, 0.3170188387650512141, 0.3333333333333333703, 0.3170188387650512141, 0.3333333333333333703, 0.3170188387650512141, 0.3333333333333333703, 0.3170188387650512141, 0.3333333333333333703, 0.3170188387650512141, 0.3333333333333333703, 0.3170188387650512141, 0.3333333333333333703, 0.3170188387650512141, 0.3333333333333333703, 0.3170188387650512141, 0.3333333333333333703, 0.3170188387650512141, 0.3333333333333333703, 0.3170188387650512141, 0.3333333333333333703, 0.3170188387650512141, 0.3333333333333333703, 0.3170188387650512141, 0.3333333333333333703, 0.3170188387650512141, 0.3333333333333333703, 0.3170188387650512141, 0.3333333333333333703, 0.3170188387650512141, 0.3333333333333333703, 0.3170188387650512141, 0.3333333333333333703, 0.3170188387650512141, 0.3333333333333333703, 0.3170188387650512141, 0.3333333333333333703, 0.3170188387650512141, 0.3333333333333333703, 0.3170188387650512141, 0.3333333333333333703, 0.3170188387650512141, 0.3333333333333333703, 0.3170188387650512141, 0.3333333333333333703, 0.3170188387650512141, 0.3333333333333333703, 0.3170188387650512141, 0.3333333333333333703, 0.3170188387650512141, 0.3333333333333333703, 0.3170188387650512141, 0.3333333333333333703, 0.3170188387650512141, 0.3333333333333333703, 0.3170188387650512141, 0.3333333333333333703, 0.3170188387650512141, 0.3333333333333333703, 0.3170188387650512141, 0.3333333333333333703, 0.3170188387650512141, 0.3333333333333333703, 0.3170188387650512141, 0.3333333333333333703, 0.3170188387650512141, 0.3333333333333333703, 0.3170188387650512141, 0.3333333333333333703, 0.3170188387650512141, 0.3333333333333333703, 0.3170188387650512141, 0.3333333333333333703, 0.3170188387650512141, 0.3333333333333333703, 0.3170188387650512141, 0.3333333333333333703, 0.3170188387650512141, 0.3333333333333333703, 0.3170188387650512141, 0.3333333333333333703, 0.3170188387650512141, 0.3333333333333333703, 0.3170188387650512141, 0.3333333333333333703, 0.3170188387650512141, 0.3333333333333333703, 0.3170188387650512141, 0.3333333333333333703, 0.3170188387650512141, 0.3333333333333333703, 0.3170188387650512141, 0.3333333333333333703, 0.3170188387650512141, 0.3333333333333333703, 0.3170188387650512141, 0.3333333333333333703, 0.3170188387650512141, 0.3333333333333333703, 0.3170188387650512141, 0.3333333333333333703, 0.3170188387650512141, 0.3333333333333333703, 0.3170188387650512141, 0.3333333333333333703, 0.3170188387650512141, 0.3333333333333333703, 0.3170188387650512141, 0.3333333333333333703, 0.3170188387650512141, 0.3333333333333333703, 0.3170188387650512141, 0.3333333333333333703, 0.3170188387650512141, 0.3333333333333333703, 0.3170188387650512141, 0.3333333333333333703, 0.3170188387650512141, 0.3333333333333333703, 0.3170188387650512141, 0.3333333333333333703, 0.3170188387650512141, 0.3333333333333333703, 0.3170188387650512141, 0.3333333333333333703, 0.3170188387650512141, 0.3333333333333333703, 0.3170188387650512141, 0.3333333333333333703, 0.3170188387650512141, 0.3333333333333333703, 0.3170188387650512141, 0.3333333333333333703, 0.3170188387650512141, 0.3333333333333333703, 0.3170188387650512141, 0.3333333333333333703, 0.3170188387650512141, 0.3333333333333333703, 0.3170188387650512141, 0.3333333333333333703, 0.3170188387650512141, 0.3333333333333333703, 0.3170188387650512141, 0.3333333333333333703, 0.3170188387650512141, 0.3333333333333333703, 0.3170188387650512141, 0.3333333333333333703, 0.3170188387650512141, 0.3333333333333333703, 0.3170188387650512141, 0.3333333333333333703, 0.3170188387650512141, 0.3333333333333333703, 0.3170188387650512141, 0.3333333333333333703, 0.3170188387650512141, 0.3333333333333333703, 0.3170188387650512141, 0.3333333333333333703, 0.3170188387650512141, 0.3333333333333333703, 0.3170188387650512141, 0.3333333333333333703, 0.3170188387650512141, 0.3333333333333333703, 0.3170188387650512141, 0.3333333333333333703, 0.3170188387650512141, 0.3333333333333333703, 0.3170188387650512141, 0.3333333333333333703, 0.3170188387650512141, 0.3333333333333333703, 0.3170188387650512141, 0.3333333333333333703, 0.3170188387650512141, 0.3333333333333333703, 0.3170188387650512141, 0.3333333333333333703, 0.3170188387650512141, 0.3333333333333333703, 0.3170188387650512141, 0.3333333333333333703, 0.3170188387650512141, 0.3333333333333333703, 0.3170188387650512141, 0.3333333333333333703),
 ( 1.000000000000000000, 0.9510565162951535312, 1.000000000000000000, 0.9510565162951535312, 1.000000000000000000, 0.9510565162951535312, 1.000000000000000000, 0.9510565162951535312, 1.000000000000000000, 0.9510565162951535312, 1.000000000000000000, 0.9510565162951535312, 1.000000000000000000, 0.9510565162951535312, 1.000000000000000000, 0.9510565162951535312, 1.000000000000000000, 0.9510565162951535312, 1.000000000000000000, 0.9510565162951535312, 1.000000000000000000, 0.9510565162951535312, 1.000000000000000000, 0.9510565162951535312, 1.000000000000000000, 0.9510565162951535312, 1.000000000000000000, 0.9510565162951535312, 1.000000000000000000, 0.9510565162951535312, 1.000000000000000000, 0.9510565162951535312, 1.000000000000000000, 0.9510565162951535312, 1.000000000000000000, 0.9510565162951535312, 1.000000000000000000, 0.9510565162951535312, 1.000000000000000000, 0.9510565162951535312, 1.000000000000000000, 0.9510565162951535312, 1.000000000000000000, 0.9510565162951535312, 1.000000000000000000, 0.9510565162951535312, 1.000000000000000000, 0.9510565162951535312, 1.000000000000000000, 0.9510565162951535312, 1.000000000000000000, 0.9510565162951535312, 1.000000000000000000, 0.9510565162951535312, 1.000000000000000000, 0.9510565162951535312, 1.000000000000000000, 0.9510565162951535312, 1.000000000000000000, 0.9510565162951535312, 1.000000000000000000, 0.9510565162951535312, 1.000000000000000000, 0.9510565162951535312, 1.000000000000000000, 0.9510565162951535312, 1.000000000000000000, 0.9510565162951535312, 1.000000000000000000, 0.9510565162951535312, 1.000000000000000000, 0.9510565162951535312, 1.000000000000000000, 0.9510565162951535312, 1.000000000000000000, 0.9510565162951535312, 1.000000000000000000, 0.9510565162951535312, 1.000000000000000000, 0.9510565162951535312, 1.000000000000000000, 0.9510565162951535312, 1.000000000000000000, 0.9510565162951535312, 1.000000000000000000, 0.9510565162951535312, 1.000000000000000000, 0.9510565162951535312, 1.000000000000000000, 0.9510565162951535312, 1.000000000000000000, 0.9510565162951535312, 1.000000000000000000, 0.9510565162951535312, 1.000000000000000000, 0.9510565162951535312, 1.000000000000000000, 0.9510565162951535312, 1.000000000000000000, 0.9510565162951535312, 1.000000000000000000, 0.9510565162951535312, 1.000000000000000000, 0.9510565162951535312, 1.000000000000000000, 0.9510565162951535312, 1.000000000000000000, 0.9510565162951535312, 1.000000000000000000, 0.9510565162951535312, 1.000000000000000000, 0.9510565162951535312, 1.000000000000000000, 0.9510565162951535312, 1.000000000000000000, 0.9510565162951535312, 1.000000000000000000, 0.9510565162951535312, 1.000000000000000000, 0.9510565162951535312, 1.000000000000000000, 0.9510565162951535312, 1.000000000000000000, 0.9510565162951535312, 1.000000000000000000, 0.9510565162951535312, 1.000000000000000000, 0.9510565162951535312, 1.000000000000000000, 0.9510565162951535312, 1.000000000000000000, 0.9510565162951535312, 1.000000000000000000, 0.9510565162951535312, 1.000000000000000000, 0.9510565162951535312, 1.000000000000000000, 0.9510565162951535312, 1.000000000000000000, 0.9510565162951535312, 1.000000000000000000, 0.9510565162951535312, 1.000000000000000000, 0.9510565162951535312, 1.000000000000000000, 0.9510565162951535312, 1.000000000000000000, 0.9510565162951535312, 1.000000000000000000, 0.9510565162951535312, 1.000000000000000000, 0.9510565162951535312, 1.000000000000000000, 0.9510565162951535312, 1.000000000000000000, 0.9510565162951535312, 1.000000000000000000, 0.9510565162951535312, 1.000000000000000000, 0.9510565162951535312, 1.000000000000000000, 0.9510565162951535312, 1.000000000000000000, 0.9510565162951535312, 1.000000000000000000, 0.9510565162951535312, 1.000000000000000000, 0.9510565162951535312, 1.000000000000000000, 0.9510565162951535312, 1.000000000000000000, 0.9510565162951535312, 1.000000000000000000, 0.9510565162951535312, 1.000000000000000000, 0.9510565162951535312, 1.000000000000000000, 0.9510565162951535312, 1.000000000000000000, 0.9510565162951535312, 1.000000000000000000, 0.9510565162951535312, 1.000000000000000000, 0.9510565162951535312, 1.000000000000000000, 0.9510565162951535312, 1.000000000000000000, 0.9510565162951535312, 1.000000000000000000, 0.9510565162951535312, 1.000000000000000000, 0.9510565162951535312, 1.000000000000000000, 0.9510565162951535312, 1.000000000000000000, 0.9510565162951535312, 1.000000000000000000, 0.9510565162951535312, 1.000000000000000000, 0.9510565162951535312, 1.000000000000000000),
 ( 0.3333333333333333703, 0.3170188387650512141, 0.3333333333333333703, 0.3170188387650512141, 0.3333333333333333703, 0.3170188387650512141, 0.3333333333333333703, 0.3170188387650512141, 0.3333333333333333703, 0.3170188387650512141, 0.3333333333333333703, 0.3170188387650512141, 0.3333333333333333703, 0.3170188387650512141, 0.3333333333333333703, 0.3170188387650512141, 0.3333333333333333703, 0.3170188387650512141, 0.3333333333333333703, 0.3170188387650512141, 0.3333333333333333703, 0.3170188387650512141, 0.3333333333333333703, 0.3170188387650512141, 0.3333333333333333703, 0.3170188387650512141, 0.3333333333333333703, 0.3170188387650512141, 0.3333333333333333703, 0.3170188387650512141, 0.3333333333333333703, 0.3170188387650512141, 0.3333333333333333703, 0.3170188387650512141, 0.3333333333333333703, 0.3170188387650512141, 0.3333333333333333703, 0.3170188387650512141, 0.3333333333333333703, 0.3170188387650512141, 0.3333333333333333703, 0.3170188387650512141, 0.3333333333333333703, 0.3170188387650512141, 0.3333333333333333703, 0.3170188387650512141, 0.3333333333333333703, 0.3170188387650512141, 0.3333333333333333703, 0.3170188387650512141, 0.3333333333333333703, 0.3170188387650512141, 0.3333333333333333703, 0.3170188387650512141, 0.3333333333333333703, 0.3170188387650512141, 0.3333333333333333703, 0.3170188387650512141, 0.3333333333333333703, 0.3170188387650512141, 0.3333333333333333703, 0.3170188387650512141, 0.3333333333333333703, 0.3170188387650512141, 0.3333333333333333703, 0.3170188387650512141, 0.3333333333333333703, 0.3170188387650512141, 0.3333333333333333703, 0.3170188387650512141, 0.3333333333333333703, 0.3170188387650512141, 0.3333333333333333703, 0.3170188387650512141, 0.3333333333333333703, 0.3170188387650512141, 0.3333333333333333703, 0.3170188387650512141, 0.3333333333333333703, 0.3170188387650512141, 0.3333333333333333703, 0.3170188387650512141, 0.3333333333333333703, 0.3170188387650512141, 0.3333333333333333703, 0.3170188387650512141, 0.3333333333333333703, 0.3170188387650512141, 0.3333333333333333703, 0.3170188387650512141, 0.3333333333333333703, 0.3170188387650512141, 0.3333333333333333703, 0.3170188387650512141, 0.3333333333333333703, 0.3170188387650512141, 0.3333333333333333703, 0.3170188387650512141, 0.3333333333333333703, 0.3170188387650512141, 0.3333333333333333703, 0.3170188387650512141, 0.3333333333333333703, 0.3170188387650512141, 0.3333333333333333703, 0.3170188387650512141, 0.3333333333333333703, 0.3170188387650512141, 0.3333333333333333703, 0.3170188387650512141, 0.3333333333333333703, 0.3170188387650512141, 0.3333333333333333703, 0.3170188387650512141, 0.3333333333333333703, 0.3170188387650512141, 0.3333333333333333703, 0.3170188387650512141, 0.3333333333333333703, 0.3170188387650512141, 0.3333333333333333703, 0.3170188387650512141, 0.3333333333333333703, 0.3170188387650512141, 0.3333333333333333703, 0.3170188387650512141, 0.3333333333333333703, 0.3170188387650512141, 0.3333333333333333703, 0.3170188387650512141, 0.3333333333333333703, 0.3170188387650512141, 0.3333333333333333703, 0.3170188387650512141, 0.3333333333333333703, 0.3170188387650512141, 0.3333333333333333703, 0.3170188387650512141, 0.3333333333333333703, 0.3170188387650512141, 0.3333333333333333703, 0.3170188387650512141, 0.3333333333333333703, 0.3170188387650512141, 0.3333333333333333703, 0.3170188387650512141, 0.3333333333333333703, 0.3170188387650512141, 0.3333333333333333703, 0.3170188387650512141, 0.3333333333333333703, 0.3170188387650512141, 0.3333333333333333703, 0.3170188387650512141, 0.3333333333333333703, 0.3170188387650512141, 0.3333333333333333703, 0.3170188387650512141, 0.3333333333333333703, 0.3170188387650512141, 0.3333333333333333703, 0.3170188387650512141, 0.3333333333333333703, 0.3170188387650512141, 0.3333333333333333703, 0.3170188387650512141, 0.3333333333333333703, 0.3170188387650512141, 0.3333333333333333703, 0.3170188387650512141, 0.3333333333333333703, 0.3170188387650512141, 0.3333333333333333703, 0.3170188387650512141, 0.3333333333333333703, 0.3170188387650512141, 0.3333333333333333703, 0.3170188387650512141, 0.3333333333333333703, 0.3170188387650512141, 0.3333333333333333703, 0.3170188387650512141, 0.3333333333333333703, 0.3170188387650512141, 0.3333333333333333703, 0.3170188387650512141, 0.3333333333333333703, 0.3170188387650512141, 0.3333333333333333703, 0.3170188387650512141, 0.3333333333333333703, 0.3170188387650512141, 0.3333333333333333703, 0.3170188387650512141, 0.3333333333333333703, 0.3170188387650512141, 0.3333333333333333703, 0.3170188387650512141, 0.3333333333333333703, 0.3170188387650512141, 0.3333333333333333703),
 ( 0.3333333333333333703, 0.3170188387650512141, 0.3333333333333333703, 0.3170188387650512141, 0.3333333333333333703, 0.3170188387650512141, 0.3333333333333333703, 0.3170188387650512141, 0.3333333333333333703, 0.3170188387650512141, 0.3333333333333333703, 0.3170188387650512141, 0.3333333333333333703, 0.3170188387650512141, 0.3333333333333333703, 0.3170188387650512141, 0.3333333333333333703, 0.3170188387650512141, 0.3333333333333333703, 0.3170188387650512141, 0.3333333333333333703, 0.3170188387650512141, 0.3333333333333333703, 0.3170188387650512141, 0.3333333333333333703, 0.3170188387650512141, 0.3333333333333333703, 0.3170188387650512141, 0.3333333333333333703, 0.3170188387650512141, 0.3333333333333333703, 0.3170188387650512141, 0.3333333333333333703, 0.3170188387650512141, 0.3333333333333333703, 0.3170188387650512141, 0.3333333333333333703, 0.3170188387650512141, 0.3333333333333333703, 0.3170188387650512141, 0.3333333333333333703, 0.3170188387650512141, 0.3333333333333333703, 0.3170188387650512141, 0.3333333333333333703, 0.3170188387650512141, 0.3333333333333333703, 0.3170188387650512141, 0.3333333333333333703, 0.3170188387650512141, 0.3333333333333333703, 0.3170188387650512141, 0.3333333333333333703, 0.3170188387650512141, 0.3333333333333333703, 0.3170188387650512141, 0.3333333333333333703, 0.3170188387650512141, 0.3333333333333333703, 0.3170188387650512141, 0.3333333333333333703, 0.3170188387650512141, 0.3333333333333333703, 0.3170188387650512141, 0.3333333333333333703, 0.3170188387650512141, 0.3333333333333333703, 0.3170188387650512141, 0.3333333333333333703, 0.3170188387650512141, 0.3333333333333333703, 0.3170188387650512141, 0.3333333333333333703, 0.3170188387650512141, 0.3333333333333333703, 0.3170188387650512141, 0.3333333333333333703, 0.3170188387650512141, 0.3333333333333333703, 0.3170188387650512141, 0.3333333333333333703, 0.3170188387650512141, 0.3333333333333333703, 0.3170188387650512141, 0.3333333333333333703, 0.3170188387650512141, 0.3333333333333333703, 0.3170188387650512141, 0.3333333333333333703, 0.3170188387650512141, 0.3333333333333333703, 0.3170188387650512141, 0.3333333333333333703, 0.3170188387650512141, 0.3333333333333333703, 0.3170188387650512141, 0.3333333333333333703, 0.3170188387650512141, 0.3333333333333333703, 0.3170188387650512141, 0.3333333333333333703, 0.3170188387650512141, 0.3333333333333333703, 0.3170188387650512141, 0.3333333333333333703, 0.3170188387650512141, 0.3333333333333333703, 0.3170188387650512141, 0.3333333333333333703, 0.3170188387650512141, 0.3333333333333333703, 0.3170188387650512141, 0.3333333333333333703, 0.3170188387650512141, 0.3333333333333333703, 0.3170188387650512141, 0.3333333333333333703, 0.3170188387650512141, 0.3333333333333333703, 0.3170188387650512141, 0.3333333333333333703, 0.3170188387650512141, 0.3333333333333333703, 0.3170188387650512141, 0.3333333333333333703, 0.3170188387650512141, 0.3333333333333333703, 0.3170188387650512141, 0.3333333333333333703, 0.3170188387650512141, 0.3333333333333333703, 0.3170188387650512141, 0.3333333333333333703, 0.3170188387650512141, 0.3333333333333333703, 0.3170188387650512141, 0.3333333333333333703, 0.3170188387650512141, 0.3333333333333333703, 0.3170188387650512141, 0.3333333333333333703, 0.3170188387650512141, 0.3333333333333333703, 0.3170188387650512141, 0.3333333333333333703, 0.3170188387650512141, 0.3333333333333333703, 0.3170188387650512141, 0.3333333333333333703, 0.3170188387650512141, 0.3333333333333333703, 0.3170188387650512141, 0.3333333333333333703, 0.3170188387650512141, 0.3333333333333333703, 0.3170188387650512141, 0.3333333333333333703, 0.3170188387650512141, 0.3333333333333333703, 0.3170188387650512141, 0.3333333333333333703, 0.3170188387650512141, 0.3333333333333333703, 0.3170188387650512141, 0.3333333333333333703, 0.3170188387650512141, 0.3333333333333333703, 0.3170188387650512141, 0.3333333333333333703, 0.3170188387650512141, 0.3333333333333333703, 0.3170188387650512141, 0.3333333333333333703, 0.3170188387650512141, 0.3333333333333333703, 0.3170188387650512141, 0.3333333333333333703, 0.3170188387650512141, 0.3333333333333333703, 0.3170188387650512141, 0.3333333333333333703, 0.3170188387650512141, 0.3333333333333333703, 0.3170188387650512141, 0.3333333333333333703, 0.3170188387650512141, 0.3333333333333333703, 0.3170188387650512141, 0.3333333333333333703, 0.3170188387650512141, 0.3333333333333333703, 0.3170188387650512141, 0.3333333333333333703, 0.3170188387650512141, 0.3333333333333333703, 0.3170188387650512141, 0.3333333333333333703, 0.3170188387650512141, 0.3333333333333333703, 0.3170188387650512141, 0.3333333333333333703),
 ( 1.000000000000000000, 0.9510565162951535312, 1.000000000000000000, 0.9510565162951535312, 1.000000000000000000, 0.9510565162951535312, 1.000000000000000000, 0.9510565162951535312, 1.000000000000000000, 0.9510565162951535312, 1.000000000000000000, 0.9510565162951535312, 1.000000000000000000, 0.9510565162951535312, 1.000000000000000000, 0.9510565162951535312, 1.000000000000000000, 0.9510565162951535312, 1.000000000000000000, 0.9510565162951535312, 1.000000000000000000, 0.9510565162951535312, 1.000000000000000000, 0.9510565162951535312, 1.000000000000000000, 0.9510565162951535312, 1.000000000000000000, 0.9510565162951535312, 1.000000000000000000, 0.9510565162951535312, 1.000000000000000000, 0.9510565162951535312, 1.000000000000000000, 0.9510565162951535312, 1.000000000000000000, 0.9510565162951535312, 1.000000000000000000, 0.9510565162951535312, 1.000000000000000000, 0.9510565162951535312, 1.000000000000000000, 0.9510565162951535312, 1.000000000000000000, 0.9510565162951535312, 1.000000000000000000, 0.9510565162951535312, 1.000000000000000000, 0.9510565162951535312, 1.000000000000000000, 0.9510565162951535312, 1.000000000000000000, 0.9510565162951535312, 1.000000000000000000, 0.9510565162951535312, 1.000000000000000000, 0.9510565162951535312, 1.000000000000000000, 0.9510565162951535312, 1.000000000000000000, 0.9510565162951535312, 1.000000000000000000, 0.9510565162951535312, 1.000000000000000000, 0.9510565162951535312, 1.000000000000000000, 0.9510565162951535312, 1.000000000000000000, 0.9510565162951535312, 1.000000000000000000, 0.9510565162951535312, 1.000000000000000000, 0.9510565162951535312, 1.000000000000000000, 0.9510565162951535312, 1.000000000000000000, 0.9510565162951535312, 1.000000000000000000, 0.9510565162951535312, 1.000000000000000000, 0.9510565162951535312, 1.000000000000000000, 0.9510565162951535312, 1.000000000000000000, 0.9510565162951535312, 1.000000000000000000, 0.9510565162951535312, 1.000000000000000000, 0.9510565162951535312, 1.000000000000000000, 0.9510565162951535312, 1.000000000000000000, 0.9510565162951535312, 1.000000000000000000, 0.9510565162951535312, 1.000000000000000000, 0.9510565162951535312, 1.000000000000000000, 0.9510565162951535312, 1.000000000000000000, 0.9510565162951535312, 1.000000000000000000, 0.9510565162951535312, 1.000000000000000000, 0.9510565162951535312, 1.000000000000000000, 0.9510565162951535312, 1.000000000000000000, 0.9510565162951535312, 1.000000000000000000, 0.9510565162951535312, 1.000000000000000000, 0.9510565162951535312, 1.000000000000000000, 0.9510565162951535312, 1.000000000000000000, 0.9510565162951535312, 1.000000000000000000, 0.9510565162951535312, 1.000000000000000000, 0.9510565162951535312, 1.000000000000000000, 0.9510565162951535312, 1.000000000000000000, 0.9510565162951535312, 1.000000000000000000, 0.9510565162951535312, 1.000000000000000000, 0.9510565162951535312, 1.000000000000000000, 0.9510565162951535312, 1.000000000000000000, 0.9510565162951535312, 1.000000000000000000, 0.9510565162951535312, 1.000000000000000000, 0.9510565162951535312, 1.000000000000000000, 0.9510565162951535312, 1.000000000000000000, 0.9510565162951535312, 1.000000000000000000, 0.9510565162951535312, 1.000000000000000000, 0.9510565162951535312, 1.000000000000000000, 0.9510565162951535312, 1.000000000000000000, 0.9510565162951535312, 1.000000000000000000, 0.9510565162951535312, 1.000000000000000000, 0.9510565162951535312, 1.000000000000000000, 0.9510565162951535312, 1.000000000000000000, 0.9510565162951535312, 1.000000000000000000, 0.9510565162951535312, 1.000000000000000000, 0.9510565162951535312, 1.000000000000000000, 0.9510565162951535312, 1.000000000000000000, 0.9510565162951535312, 1.000000000000000000, 0.9510565162951535312, 1.000000000000000000, 0.9510565162951535312, 1.000000000000000000, 0.9510565162951535312, 1.000000000000000000, 0.9510565162951535312, 1.000000000000000000, 0.9510565162951535312, 1.000000000000000000, 0.9510565162951535312, 1.000000000000000000, 0.9510565162951535312, 1.000000000000000000, 0.9510565162951535312, 1.000000000000000000, 0.9510565162951535312, 1.000000000000000000, 0.9510565162951535312, 1.000000000000000000, 0.9510565162951535312, 1.000000000000000000, 0.9510565162951535312, 1.000000000000000000, 0.9510565162951535312, 1.000000000000000000, 0.9510565162951535312, 1.000000000000000000, 0.9510565162951535312, 1.000000000000000000, 0.9510565162951535312, 1.000000000000000000, 0.9510565162951535312, 1.000000000000000000, 0.9510565162951535312, 1.000000000000000000) ) ) 
 REPRESENTATION_ITEM ( '' )  SURFACE ( )  );
#9362 = CARTESIAN_POINT ( 'NONE',  ( 0.1217565302851118803, -3.710888496608922171, 0.5725525826504672677 ) ) ;
#9363 = DIRECTION ( 'NONE',  ( 0.000000000000000000, 0.000000000000000000, 1.000000000000000000 ) ) ;
#9364 = PLANE ( 'NONE',  #1121 ) ;
#9365 = CARTESIAN_POINT ( 'NONE',  ( 45.86712807150323812, 65.29948385550241596, -5.649768623646098220 ) ) ;
#9366 = CARTESIAN_POINT ( 'NONE',  ( 56.65037692655918988, 59.89948385550241028, -2.184720259617163762 ) ) ;
#9367 = CARTESIAN_POINT ( 'NONE',  ( 45.90387839640208512, 62.30051614449766362, -5.676469297603124353 ) ) ;
#9368 = CARTESIAN_POINT ( 'NONE',  ( 2.500000000000000888, 3.061616997868384127E-16, -4.974599999999998801 ) ) ;
#9369 = FACE_OUTER_BOUND ( 'NONE', #13294, .T. ) ;
#9370 = FACE_OUTER_BOUND ( 'NONE', #7945, .T. ) ;
#9371 = CARTESIAN_POINT ( 'NONE',  ( 45.90387839640208512, 50.30051614449766362, -5.676469297603124353 ) ) ;
#9372 = CARTESIAN_POINT ( 'NONE',  ( 50.02271294988511841, 50.49948385550239749, 6.000000000000000888 ) ) ;
#9373 = LINE ( 'NONE', #7439, #9812 ) ;
#9374 = CIRCLE ( 'NONE', #4082, 1.500000000000001332 ) ;
#9375 = ORIENTED_EDGE ( 'NONE', *, *, #13349, .T. ) ;
#9376 = DIRECTION ( 'NONE',  ( 1.000000000000000000, 0.000000000000000000, 0.000000000000000000 ) ) ;
#9377 = VERTEX_POINT ( 'NONE', #803 ) ;
#9378 = AXIS2_PLACEMENT_3D ( 'NONE', #1207, #7655, #11860 ) ;
#9379 = ORIENTED_EDGE ( 'NONE', *, *, #497, .T. ) ;
#9380 = CARTESIAN_POINT ( 'NONE',  ( 4.071447262713888016, -2.020725942163694722, -3.499999999999999556 ) ) ;
#9381 = CARTESIAN_POINT ( 'NONE',  ( 6.242800618755075526, 3.923709308887314950, -3.414402460853798171 ) ) ;
#9382 = AXIS2_PLACEMENT_3D ( 'NONE', #5660, #9927, #640 ) ;
#9383 = CARTESIAN_POINT ( 'NONE',  ( 6.323279575528418128, -5.335162385627848280, -0.7592276814619393077 ) ) ;
#9384 =( LENGTH_UNIT ( ) NAMED_UNIT ( * ) SI_UNIT ( .MILLI., .METRE. ) );
#9385 = CARTESIAN_POINT ( 'NONE',  ( 52.25172492374522903, 45.59948385550240602, -7.007379884777225953 ) ) ;
#9386 = ADVANCED_FACE ( 'NONE', ( #5954 ), #588, .F. ) ;
#9387 = VECTOR ( 'NONE', #12393, 1000.000000000000000 ) ;
#9388 = CARTESIAN_POINT ( 'NONE',  ( -4.175648173966055587, 2.207990556236529844, -3.469390959564062626 ) ) ;
#9389 = CARTESIAN_POINT ( 'NONE',  ( 48.07319477248762496, 48.40051614449766504, -6.007379884777208190 ) ) ;
#9390 = CARTESIAN_POINT ( 'NONE',  ( 4.071447262713890680, -4.041451884327386779, 0.000000000000000000 ) ) ;
#9391 = B_SPLINE_CURVE_WITH_KNOTS ( 'NONE', 3,
 ( #8245, #9545, #954, #12515 ),
 .UNSPECIFIED., .F., .F.,
 ( 4, 4 ),
 ( 0.000000000000000000, 0.002452478801916361129 ),
 .UNSPECIFIED. ) ;
#9392 = VECTOR ( 'NONE', #8354, 1000.000000000000000 ) ;
#9393 = CARTESIAN_POINT ( 'NONE',  ( 6.367873360227556567, 2.886751345948125991, 4.999999999999999112 ) ) ;
#9394 = CARTESIAN_POINT ( 'NONE',  ( 49.97728705011488159, 51.49948385550240459, -7.000000000000000888 ) ) ;
#9395 = ORIENTED_EDGE ( 'NONE', *, *, #6073, .T. ) ;
#9396 = CARTESIAN_POINT ( 'NONE',  ( 50.02271294988512551, 52.49948385550240459, 7.000000000000000888 ) ) ;
#9397 = VECTOR ( 'NONE', #12158, 1000.000000000000000 ) ;
#9398 = EDGE_LOOP ( 'NONE', ( #2399, #12773, #9757, #4382 ) ) ;
#9399 = CARTESIAN_POINT ( 'NONE',  ( 4.033906725095553369, -1.419670120619691334, 3.500000000000000444 ) ) ;
#9400 = DIRECTION ( 'NONE',  ( 0.000000000000000000, 0.000000000000000000, -1.000000000000000000 ) ) ;
#9401 = DIRECTION ( 'NONE',  ( -1.000000000000000000, 0.000000000000000000, 0.000000000000000000 ) ) ;
#9402 = DIRECTION ( 'NONE',  ( 0.000000000000000000, -0.000000000000000000, 1.000000000000000000 ) ) ;
#9403 = CARTESIAN_POINT ( 'NONE',  ( 56.66441430157294690, 46.90051614449765793, -2.141517661632166281 ) ) ;
#9404 = CARTESIAN_POINT ( 'NONE',  ( 6.244004651191001010, -4.178905357954647570, 2.972460101650454600 ) ) ;
#9405 = CARTESIAN_POINT ( 'NONE',  ( 52.57664461997811856, 63.59948385550239891, -8.007379884777229506 ) ) ;
#9406 = DIRECTION ( 'NONE',  ( 1.000000000000000000, 0.000000000000000000, 0.000000000000000000 ) ) ;
#9407 = CARTESIAN_POINT ( 'NONE',  ( 54.68390685589033495, 57.69948385550241454, -6.485486291978119766 ) ) ;
#9408 = ORIENTED_EDGE ( 'NONE', *, *, #13588, .F. ) ;
#9409 = EDGE_LOOP ( 'NONE', ( #423, #7569 ) ) ;
#9410 = CARTESIAN_POINT ( 'NONE',  ( 4.000000000000000000, 3.500000000000000000, 0.000000000000000000 ) ) ;
#9411 = ADVANCED_FACE ( 'NONE', ( #12227 ), #9114, .F. ) ;
#9412 = B_SPLINE_CURVE_WITH_KNOTS ( 'NONE', 3,
 ( #2797, #1744, #5915, #4804, #4949, #9162 ),
 .UNSPECIFIED., .F., .F.,
 ( 4, 2, 4 ),
 ( 0.002044882221487539717, 0.003063384235218500652, 0.004081886248949461587 ),
 .UNSPECIFIED. ) ;
#9413 = EDGE_CURVE ( 'NONE', #5998, #12021, #195, .T. ) ;
#9414 = DIRECTION ( 'NONE',  ( -1.000000000000000000, 0.000000000000000000, 0.000000000000000000 ) ) ;
#9415 = CARTESIAN_POINT ( 'NONE',  ( 6.355324643801638196, 1.972141403783284730, -5.108685331087993831 ) ) ;
#9416 = CARTESIAN_POINT ( 'NONE',  ( 50.02271294988506156, 46.50051614449766646, -6.000000000000000888 ) ) ;
#9417 = EDGE_CURVE ( 'NONE', #4712, #6427, #9773, .T. ) ;
#9418 = CARTESIAN_POINT ( 'NONE',  ( 47.70284917648459810, 61.60051614449765367, 6.992620115222797139 ) ) ;
#9419 = CARTESIAN_POINT ( 'NONE',  ( 50.02271294988513972, 46.49948385550240459, 8.000000000000001776 ) ) ;
#9420 = CARTESIAN_POINT ( 'NONE',  ( 4.071447262713887127, 2.020725942163688504, 3.500000000000000000 ) ) ;
#9421 = CARTESIAN_POINT ( 'NONE',  ( 58.41169779390614281, 51.00051614449765935, 0.02388180880515032231 ) ) ;
#9422 = ORIENTED_EDGE ( 'NONE', *, *, #2529, .T. ) ;
#9423 = CIRCLE ( 'NONE', #1453, 8.099999999999999645 ) ;
#9424 = VERTEX_POINT ( 'NONE', #6101 ) ;
#9425 = ORIENTED_EDGE ( 'NONE', *, *, #8230, .T. ) ;
#9426 = CARTESIAN_POINT ( 'NONE',  ( 6.534224484704327374, 5.901860969583204941, 2.029550679094937724E-14 ) ) ;
#9427 = CARTESIAN_POINT ( 'NONE',  ( 1.171083334267915221, -24.65495046420793201, 9.999999999999998224 ) ) ;
#9428 = CARTESIAN_POINT ( 'NONE',  ( 3.951447005078450037, -1.347150628109123893, 3.500000000000000888 ) ) ;
#9429 = CARTESIAN_POINT ( 'NONE',  ( 44.88205777487398507, 53.19948385550240744, -3.688883143319540814 ) ) ;
#9430 = DIRECTION ( 'NONE',  ( 0.000000000000000000, 1.224646799147353207E-16, 1.000000000000000000 ) ) ;
#9431 = CARTESIAN_POINT ( 'NONE',  ( 45.90387839640208512, 60.30051614449766362, -5.676469297603124353 ) ) ;
#9432 = PLANE ( 'NONE',  #471 ) ;
#9433 = CARTESIAN_POINT ( 'NONE',  ( -74.99999999999997158, 32.50000000000001421, 15.00000000000000000 ) ) ;
#9434 = CARTESIAN_POINT ( 'NONE',  ( 52.07576163693497051, 45.00000000000001421, -7.275735003127095979 ) ) ;
#9435 = CARTESIAN_POINT ( 'NONE',  ( 54.13287192849671214, 52.70051614449766220, -5.649768623646139964 ) ) ;
#9436 = CARTESIAN_POINT ( 'NONE',  ( 53.50833635130540955, 57.69948385550241454, -4.867452303228209765 ) ) ;
#9437 = CARTESIAN_POINT ( 'NONE',  ( 55.32279841668061238, 44.85244137215321558, -4.999999999999997335 ) ) ;
#9438 = VERTEX_POINT ( 'NONE', #10294 ) ;
#9439 = FACE_OUTER_BOUND ( 'NONE', #11023, .T. ) ;
#9440 = ORIENTED_EDGE ( 'NONE', *, *, #5741, .T. ) ;
#9441 = CARTESIAN_POINT ( 'NONE',  ( 6.403457969954081008, 2.888443235695449030, 5.002930439003169028 ) ) ;
#9442 = CARTESIAN_POINT ( 'NONE',  ( 0.000000000000000000, 0.000000000000000000, 0.000000000000000000 ) ) ;
#9443 = EDGE_CURVE ( 'NONE', #9655, #12675, #5332, .T. ) ;
#9444 = CARTESIAN_POINT ( 'NONE',  ( 6.362382503762741948, -2.018850626433581041, 5.108861885121540602 ) ) ;
#9445 =( NAMED_UNIT ( * ) SI_UNIT ( $, .STERADIAN. ) SOLID_ANGLE_UNIT ( ) );
#9446 = CARTESIAN_POINT ( 'NONE',  ( 0.000000000000000000, 0.000000000000000000, 0.000000000000000000 ) ) ;
#9447 = LINE ( 'NONE', #11532, #7076 ) ;
#9448 = CARTESIAN_POINT ( 'NONE',  ( 44.30067958973594955, 54.10051614449766078, -1.875703265242155693 ) ) ;
#9449 = DIRECTION ( 'NONE',  ( 0.000000000000000000, 0.000000000000000000, 1.000000000000000000 ) ) ;
#9450 = CARTESIAN_POINT ( 'NONE',  ( 2.449293598294706513E-15, -20.00000000000000000, -9.000000000000000000 ) ) ;
#9451 = CARTESIAN_POINT ( 'NONE',  ( 49.97728705011488159, 63.49948385550241170, -7.000000000000000888 ) ) ;
#9452 = CARTESIAN_POINT ( 'NONE',  ( 49.97728705011488159, 61.49948385550240459, -7.000000000000000888 ) ) ;
#9453 = ORIENTED_EDGE ( 'NONE', *, *, #9122, .F. ) ;
#9454 = PRODUCT_DEFINITION ( 'UNKNOWN', '', #8831, #7589 ) ;
#9455 = ORIENTED_EDGE ( 'NONE', *, *, #1135, .T. ) ;
#9456 = CARTESIAN_POINT ( 'NONE',  ( 32.49999999999998579, 45.00000000000001421, 5.000000000000003553 ) ) ;
#9457 = CARTESIAN_POINT ( 'NONE',  ( -20.00000000000000000, -19.99999999999999289, -20.00000000000000000 ) ) ;
#9458 = DIRECTION ( 'NONE',  ( -0.000000000000000000, -0.000000000000000000, 1.000000000000000000 ) ) ;
#9459 = DIRECTION ( 'NONE',  ( -0.000000000000000000, -0.000000000000000000, 1.000000000000000000 ) ) ;
#9460 = FACE_OUTER_BOUND ( 'NONE', #3684, .T. ) ;
#9461 = CARTESIAN_POINT ( 'NONE',  ( 45.86712807150329496, 49.70051614449766220, 5.649768623646139964 ) ) ;
#9462 = AXIS2_PLACEMENT_3D ( 'NONE', #2891, #7191, #6158 ) ;
#9463 = PLANE ( 'NONE',  #9280 ) ;
#9464 = CARTESIAN_POINT ( 'NONE',  ( 55.94051828345050836, 47.79948385550240886, -4.345558710429104465 ) ) ;
#9465 = COLOUR_RGB ( '',1.000000000000000000, 0.9490196078431372140, 0.9098039215686274384 ) ;
#9466 = CARTESIAN_POINT ( 'NONE',  ( 56.79116909180255135, 57.79948385550240175, -4.963592699179005585 ) ) ;
#9467 = ADVANCED_FACE ( 'NONE', ( #4212 ), #10435, .T. ) ;
#9468 = VERTEX_POINT ( 'NONE', #874 ) ;
#9469 = ORIENTED_EDGE ( 'NONE', *, *, #2290, .F. ) ;
#9470 = AXIS2_PLACEMENT_3D ( 'NONE', #9239, #13297, #7171 ) ;
#9471 = CARTESIAN_POINT ( 'NONE',  ( 54.42198456365324688, 44.83981687677464834, -4.999999999999773515 ) ) ;
#9472 = AXIS2_PLACEMENT_3D ( 'NONE', #1820, #13290, #6066 ) ;
#9473 = DIRECTION ( 'NONE',  ( -0.000000000000000000, -0.000000000000000000, -1.000000000000000000 ) ) ;
#9474 = PLANE ( 'NONE',  #9297 ) ;
#9475 = CARTESIAN_POINT ( 'NONE',  ( -3.309651814758565180, -5.455921364805393026, -1.000000000000000000 ) ) ;
#9476 = CARTESIAN_POINT ( 'NONE',  ( 53.50833635130544508, 49.30051614449766362, 4.867452303228181343 ) ) ;
#9477 = CARTESIAN_POINT ( 'NONE',  ( 47.74827507625470702, 58.40051614449766504, -7.007379884777204637 ) ) ;
#9478 = EDGE_CURVE ( 'NONE', #11144, #2434, #630, .T. ) ;
#9479 = CARTESIAN_POINT ( 'NONE',  ( 43.20883090819745576, 46.79948385550240886, 4.963592699179006473 ) ) ;
#9480 = CARTESIAN_POINT ( 'NONE',  ( 4.000000000000001776, 2.694222958124178486E-16, 2.200000000000001066 ) ) ;
#9481 = EDGE_CURVE ( 'NONE', #12594, #10838, #2005, .T. ) ;
#9482 = CARTESIAN_POINT ( 'NONE',  ( 54.68390685589039890, 59.30051614449766362, 6.485486291978072693 ) ) ;
#9483 = EDGE_CURVE ( 'NONE', #6478, #2588, #5747, .T. ) ;
#9484 = ORIENTED_EDGE ( 'NONE', *, *, #9911, .F. ) ;
#9485 = ORIENTED_EDGE ( 'NONE', *, *, #11005, .F. ) ;
#9486 = VERTEX_POINT ( 'NONE', #9604 ) ;
#9487 =( GEOMETRIC_REPRESENTATION_CONTEXT ( 3 ) GLOBAL_UNCERTAINTY_ASSIGNED_CONTEXT ( ( #11862 ) ) GLOBAL_UNIT_ASSIGNED_CONTEXT ( ( #5506, #8612, #11716 ) ) REPRESENTATION_CONTEXT ( 'NONE', 'WORKASPACE' ) );
#9488 = CARTESIAN_POINT ( 'NONE',  ( 6.420058897733093239, 5.782965130189194447, -1.451745169709246731E-16 ) ) ;
#9490 = CIRCLE ( 'NONE', #5310, 2.649999999999988365 ) ;
#9489 = CARTESIAN_POINT ( 'NONE',  ( 6.534224484704323821, 2.950930484791612685, -5.111161529262899350 ) ) ;
#9491 = DIRECTION ( 'NONE',  ( 1.000000000000000000, 0.000000000000000000, 0.000000000000000000 ) ) ;
#9492 = CARTESIAN_POINT ( 'NONE',  ( -11.49038105676654453, -27.50000000000006040, -9.000000000000000000 ) ) ;
#9493 = CARTESIAN_POINT ( 'NONE',  ( 55.11794222512601493, 50.19948385550241454, 3.688883143319541702 ) ) ;
#9494 = AXIS2_PLACEMENT_3D ( 'NONE', #10277, #2152, #8528 ) ;
#9495 = CARTESIAN_POINT ( 'NONE',  ( 47.74827507625477807, 62.59948385550239891, 7.007379884777229506 ) ) ;
#9496 = CARTESIAN_POINT ( 'NONE',  ( 42.63976443033212860, 64.00051614449765225, -0.02388180880514948964 ) ) ;
#9497 = LINE ( 'NONE', #2093, #8668 ) ;
#9498 = LINE ( 'NONE', #9433, #3453 ) ;
#9499 = EDGE_CURVE ( 'NONE', #6494, #11878, #9533, .T. ) ;
#9500 = DIRECTION ( 'NONE',  ( -1.000000000000000000, -0.000000000000000000, -0.000000000000000000 ) ) ;
#9501 = CARTESIAN_POINT ( 'NONE',  ( 54.09612160359792199, 55.30051614449765651, 5.676469297603124353 ) ) ;
#9502 = STYLED_ITEM ( 'NONE', ( #11559 ), #11781 ) ;
#9503 = CARTESIAN_POINT ( 'NONE',  ( 44.30067958973596376, 56.89948385550240317, 1.875703265242204099 ) ) ;
#9504 = VECTOR ( 'NONE', #7668, 1000.000000000000000 ) ;
#9505 = CARTESIAN_POINT ( 'NONE',  ( -12.17636723815382993, -11.24008670809956456, 9.000000000000000000 ) ) ;
#9506 = EDGE_CURVE ( 'NONE', #10021, #7078, #4867, .T. ) ;
#9507 = EDGE_LOOP ( 'NONE', ( #5923, #1630, #2978, #2333 ) ) ;
#9508 = DIRECTION ( 'NONE',  ( 0.000000000000000000, 0.5000000000000007772, -0.8660254037844381525 ) ) ;
#9509 = EDGE_LOOP ( 'NONE', ( #11407, #13094 ) ) ;
#9510 = CARTESIAN_POINT ( 'NONE',  ( 6.367873360227556567, 2.886751345948125991, 4.999999999999999112 ) ) ;
#9511 = LINE ( 'NONE', #12809, #13132 ) ;
#9512 = FACE_OUTER_BOUND ( 'NONE', #2538, .T. ) ;
#9513 = CARTESIAN_POINT ( 'NONE',  ( 55.94051828345050836, 51.79948385550240175, -4.345558710429104465 ) ) ;
#9514 = CIRCLE ( 'NONE', #12, 1.500000000000001110 ) ;
#9515 = DIRECTION ( 'NONE',  ( -0.000000000000000000, -0.000000000000000000, -1.000000000000000000 ) ) ;
#9516 = CARTESIAN_POINT ( 'NONE',  ( 50.02271294988506156, 54.50051614449765935, -6.000000000000000888 ) ) ;
#9517 = DIRECTION ( 'NONE',  ( 0.000000000000000000, 0.000000000000000000, 1.000000000000000000 ) ) ;
#9518 = DIRECTION ( 'NONE',  ( 1.000000000000000000, 0.000000000000000000, 0.000000000000000000 ) ) ;
#9519 = EDGE_CURVE ( 'NONE', #686, #11745, #5327, .T. ) ;
#9520 = CARTESIAN_POINT ( 'NONE',  ( 50.02271294988512551, 60.49948385550240459, 7.000000000000000888 ) ) ;
#9521 = CARTESIAN_POINT ( 'NONE',  ( 50.02271294988512551, 60.49948385550240459, 7.000000000000000888 ) ) ;
#9522 = ADVANCED_FACE ( 'NONE', ( #6370 ), #9463, .F. ) ;
#9523 = VERTEX_POINT ( 'NONE', #3244 ) ;
#9524 = CONICAL_SURFACE ( 'NONE', #6240, 5.560781378645573980, 1.221730476396046816 ) ;
#9525 = VERTEX_POINT ( 'NONE', #6242 ) ;
#9526 = FACE_BOUND ( 'NONE', #8204, .T. ) ;
#9527 = DIRECTION ( 'NONE',  ( 0.03086419753086420623, 0.9995235871707959241, -0.000000000000000000 ) ) ;
#9528 = CARTESIAN_POINT ( 'NONE',  ( 1.000000000000000000, -14.00000000000000000, 8.999999999999998224 ) ) ;
#9529 = DIRECTION ( 'NONE',  ( -1.000000000000000000, 0.000000000000000000, -0.000000000000000000 ) ) ;
#9530 = CARTESIAN_POINT ( 'NONE',  ( 43.34962307344081012, 46.89948385550240317, 2.184720259617164650 ) ) ;
#9531 = CONICAL_SURFACE ( 'NONE', #8872, 1.610000000000000098, 0.7853981633974658205 ) ;
#9532 = CARTESIAN_POINT ( 'NONE',  ( 44.03140696652198471, 49.80051614449766362, 4.306917132069485454 ) ) ;
#9533 = LINE ( 'NONE', #8435, #11490 ) ;
#9534 = AXIS2_PLACEMENT_3D ( 'NONE', #11672, #7670, #11874 ) ;
#9535 = CARTESIAN_POINT ( 'NONE',  ( 54.13287192849676188, 48.29948385550240175, 5.649768623646098220 ) ) ;
#9536 = LINE ( 'NONE', #11614, #2683 ) ;
#9537 = CARTESIAN_POINT ( 'NONE',  ( 54.68390685589033495, 59.69948385550240744, -6.485486291978119766 ) ) ;
#9538 = EDGE_LOOP ( 'NONE', ( #10803, #1356 ) ) ;
#9539 = ORIENTED_EDGE ( 'NONE', *, *, #6489, .T. ) ;
#9540 = CIRCLE ( 'NONE', #3364, 1.500000000000000222 ) ;
#9541 = VECTOR ( 'NONE', #4891, 1000.000000000000000 ) ;
#9542 = ADVANCED_FACE ( 'NONE', ( #10565 ), #5198, .F. ) ;
#9543 = CARTESIAN_POINT ( 'NONE',  ( 3.951447005078450925, 2.357513599190970144, 2.916666666666667407 ) ) ;
#9544 = CARTESIAN_POINT ( 'NONE',  ( -74.99999999999997158, 40.00000000000001421, -10.00000000000000000 ) ) ;
#9545 = CARTESIAN_POINT ( 'NONE',  ( 4.203833317240879275, 1.627343821129582979, -3.597273115243889929 ) ) ;
#9546 = CARTESIAN_POINT ( 'NONE',  ( -1.498123826657861368, -34.92499999999999716, 9.000000000000000000 ) ) ;
#9547 = CARTESIAN_POINT ( 'NONE',  ( 43.69122665457040000, 46.00051614449764514, -0.02388180880515696977 ) ) ;
#9548 = CARTESIAN_POINT ( 'NONE',  ( 47.70284917648459810, 57.60051614449765367, 6.992620115222797139 ) ) ;
#9549 = ADVANCED_FACE ( 'NONE', ( #3105, #13530 ), #4077, .T. ) ;
#9550 = CARTESIAN_POINT ( 'NONE',  ( 50.02271294988505446, 62.50051614449767357, -8.000000000000001776 ) ) ;
#9551 = CARTESIAN_POINT ( 'NONE',  ( 8.500000000000000000, 5.773502691896261751, 0.000000000000000000 ) ) ;
#9552 = CARTESIAN_POINT ( 'NONE',  ( 42.39856655714564226, 54.10051614449766078, -2.493737253992044156 ) ) ;
#9553 = ORIENTED_EDGE ( 'NONE', *, *, #272, .F. ) ;
#9554 =( BOUNDED_CURVE ( )  B_SPLINE_CURVE ( 2, ( #12571, #11469, #2968, #6239, #3102, #7399, #7334, #872, #6163, #3033, #1008, #10433, #8499, #1072, #9530, #10362, #2123, #11610, #8299, #6368, #11547, #13454, #5324, #5261, #12702, #4002, #58, #7195, #11398, #2060, #5123, #12499, #13661, #13526, #4210, #4279, #4073, #3242, #11665, #6099, #3760, #7665, #6563, #9015, #125, #4548, #6875, #12764, #12831, #3443, #4346, #6434, #10633, #11869, #13213, #10828, #5522, #2390, #187, #11084, #3307, #7734, #6631, #8562, #7529, #1345, #8768, #3374, #1600, #4477, #5592, #7983, #2190, #7598, #11803, #11736, #5846, #12962, #3509, #1275, #10763, #12898, #2325, #9736, #1147, #5397, #8700, #11939, #5463, #9802, #321, #2254, #9601, #2458, #253, #10044, #557, #6503, #10703, #1216, #4802, #9666, #4411, #8630, #11295, #3895, #622, #8123, #6063, #831, #1817, #7012, #8055, #9159, #7158, #13354, #908, #3002, #1956, #12262, #8263, #12327, #10190, #8194, #6199, #11153, #12466, #11367, #5161, #2723, #13490, #6945, #3831, #2862, #1671, #698, #6131, #1743, #12397, #4041, #2795, #13422, #10257, #4875, #9366, #3964, #7085, #13565, #10113, #5088, #7230, #9088, #768, #2935, #13287, #5914, #11222, #1888, #4111, #10327, #5020, #12195, #9226, #9296, #10396, #11430, #5988, #4948, #10462, #8530, #1179, #9495, #3339, #10601, #7494, #9698, #223, #18, #5292, #13627, #7563, #11638, #4243, #4311, #4175, #5360, #8462, #2155, #3066, #8335, #1108, #156, #11576, #11699, #9566, #8398, #1241, #12666, #4373, #10730, #6467 ),
 .UNSPECIFIED., .F., .F. ) 
 B_SPLINE_CURVE_WITH_KNOTS ( ( 3, 2, 2, 2, 2, 2, 2, 2, 2, 2, 2, 2, 2, 2, 2, 2, 2, 2, 2, 2, 2, 2, 2, 2, 2, 2, 2, 2, 2, 2, 2, 2, 2, 2, 2, 2, 2, 2, 2, 2, 2, 2, 2, 2, 2, 2, 2, 2, 2, 2, 2, 2, 2, 2, 2, 2, 2, 2, 2, 2, 2, 2, 2, 2, 2, 2, 2, 2, 2, 2, 2, 2, 2, 2, 2, 2, 2, 2, 2, 2, 2, 2, 2, 2, 2, 2, 2, 2, 2, 2, 2, 2, 2, 2, 2, 2, 2, 2, 2, 2, 3 ),
 ( 0.000000000000000000, 0.01000000000000000021, 0.02000000000000000042, 0.02999999999999999889, 0.04000000000000000083, 0.05000000000000000278, 0.05999999999999999778, 0.07000000000000000666, 0.08000000000000000167, 0.08999999999999999667, 0.1000000000000000056, 0.1100000000000000006, 0.1199999999999999956, 0.1300000000000000044, 0.1400000000000000133, 0.1499999999999999944, 0.1600000000000000033, 0.1700000000000000122, 0.1799999999999999933, 0.1900000000000000022, 0.2000000000000000111, 0.2099999999999999922, 0.2200000000000000011, 0.2300000000000000100, 0.2399999999999999911, 0.2500000000000000000, 0.2600000000000000089, 0.2700000000000000178, 0.2800000000000000266, 0.2899999999999999800, 0.2999999999999999889, 0.3099999999999999978, 0.3200000000000000067, 0.3300000000000000155, 0.3400000000000000244, 0.3499999999999999778, 0.3599999999999999867, 0.3699999999999999956, 0.3800000000000000044, 0.3900000000000000133, 0.4000000000000000222, 0.4099999999999999756, 0.4199999999999999845, 0.4299999999999999933, 0.4400000000000000022, 0.4500000000000000111, 0.4600000000000000200, 0.4699999999999999734, 0.4799999999999999822, 0.4899999999999999911, 0.5000000000000000000, 0.5100000000000000089, 0.5200000000000000178, 0.5300000000000000266, 0.5400000000000000355, 0.5500000000000000444, 0.5600000000000000533, 0.5699999999999999512, 0.5799999999999999600, 0.5899999999999999689, 0.5999999999999999778, 0.6099999999999999867, 0.6199999999999999956, 0.6300000000000000044, 0.6400000000000000133, 0.6500000000000000222, 0.6600000000000000311, 0.6700000000000000400, 0.6800000000000000488, 0.6899999999999999467, 0.6999999999999999556, 0.7099999999999999645, 0.7199999999999999734, 0.7299999999999999822, 0.7399999999999999911, 0.7500000000000000000, 0.7600000000000000089, 0.7700000000000000178, 0.7800000000000000266, 0.7900000000000000355, 0.8000000000000000444, 0.8100000000000000533, 0.8199999999999999512, 0.8299999999999999600, 0.8399999999999999689, 0.8499999999999999778, 0.8599999999999999867, 0.8699999999999999956, 0.8800000000000000044, 0.8900000000000000133, 0.9000000000000000222, 0.9100000000000000311, 0.9200000000000000400, 0.9300000000000000488, 0.9399999999999999467, 0.9499999999999999556, 0.9599999999999999645, 0.9699999999999999734, 0.9799999999999999822, 0.9899999999999999911, 1.000000000000000000 ),
 .UNSPECIFIED. ) 
 CURVE ( )  GEOMETRIC_REPRESENTATION_ITEM ( )  RATIONAL_B_SPLINE_CURVE ( ( 1.000000000000000000, 0.9510565162951535312, 1.000000000000000000, 0.9510565162951535312, 1.000000000000000000, 0.9510565162951535312, 1.000000000000000000, 0.9510565162951535312, 1.000000000000000000, 0.9510565162951535312, 1.000000000000000000, 0.9510565162951535312, 1.000000000000000000, 0.9510565162951535312, 1.000000000000000000, 0.9510565162951535312, 1.000000000000000000, 0.9510565162951535312, 1.000000000000000000, 0.9510565162951535312, 1.000000000000000000, 0.9510565162951535312, 1.000000000000000000, 0.9510565162951535312, 1.000000000000000000, 0.9510565162951535312, 1.000000000000000000, 0.9510565162951535312, 1.000000000000000000, 0.9510565162951535312, 1.000000000000000000, 0.9510565162951535312, 1.000000000000000000, 0.9510565162951535312, 1.000000000000000000, 0.9510565162951535312, 1.000000000000000000, 0.9510565162951535312, 1.000000000000000000, 0.9510565162951535312, 1.000000000000000000, 0.9510565162951535312, 1.000000000000000000, 0.9510565162951535312, 1.000000000000000000, 0.9510565162951535312, 1.000000000000000000, 0.9510565162951535312, 1.000000000000000000, 0.9510565162951535312, 1.000000000000000000, 0.9510565162951535312, 1.000000000000000000, 0.9510565162951535312, 1.000000000000000000, 0.9510565162951535312, 1.000000000000000000, 0.9510565162951535312, 1.000000000000000000, 0.9510565162951535312, 1.000000000000000000, 0.9510565162951535312, 1.000000000000000000, 0.9510565162951535312, 1.000000000000000000, 0.9510565162951535312, 1.000000000000000000, 0.9510565162951535312, 1.000000000000000000, 0.9510565162951535312, 1.000000000000000000, 0.9510565162951535312, 1.000000000000000000, 0.9510565162951535312, 1.000000000000000000, 0.9510565162951535312, 1.000000000000000000, 0.9510565162951535312, 1.000000000000000000, 0.9510565162951535312, 1.000000000000000000, 0.9510565162951535312, 1.000000000000000000, 0.9510565162951535312, 1.000000000000000000, 0.9510565162951535312, 1.000000000000000000, 0.9510565162951535312, 1.000000000000000000, 0.9510565162951535312, 1.000000000000000000, 0.9510565162951535312, 1.000000000000000000, 0.9510565162951535312, 1.000000000000000000, 0.9510565162951535312, 1.000000000000000000, 0.9510565162951535312, 1.000000000000000000, 0.9510565162951535312, 1.000000000000000000, 0.9510565162951535312, 1.000000000000000000, 0.9510565162951535312, 1.000000000000000000, 0.9510565162951535312, 1.000000000000000000, 0.9510565162951535312, 1.000000000000000000, 0.9510565162951535312, 1.000000000000000000, 0.9510565162951535312, 1.000000000000000000, 0.9510565162951535312, 1.000000000000000000, 0.9510565162951535312, 1.000000000000000000, 0.9510565162951535312, 1.000000000000000000, 0.9510565162951535312, 1.000000000000000000, 0.9510565162951535312, 1.000000000000000000, 0.9510565162951535312, 1.000000000000000000, 0.9510565162951535312, 1.000000000000000000, 0.9510565162951535312, 1.000000000000000000, 0.9510565162951535312, 1.000000000000000000, 0.9510565162951535312, 1.000000000000000000, 0.9510565162951535312, 1.000000000000000000, 0.9510565162951535312, 1.000000000000000000, 0.9510565162951535312, 1.000000000000000000, 0.9510565162951535312, 1.000000000000000000, 0.9510565162951535312, 1.000000000000000000, 0.9510565162951535312, 1.000000000000000000, 0.9510565162951535312, 1.000000000000000000, 0.9510565162951535312, 1.000000000000000000, 0.9510565162951535312, 1.000000000000000000, 0.9510565162951535312, 1.000000000000000000, 0.9510565162951535312, 1.000000000000000000, 0.9510565162951535312, 1.000000000000000000, 0.9510565162951535312, 1.000000000000000000, 0.9510565162951535312, 1.000000000000000000, 0.9510565162951535312, 1.000000000000000000, 0.9510565162951535312, 1.000000000000000000, 0.9510565162951535312, 1.000000000000000000, 0.9510565162951535312, 1.000000000000000000, 0.9510565162951535312, 1.000000000000000000, 0.9510565162951535312, 1.000000000000000000, 0.9510565162951535312, 1.000000000000000000, 0.9510565162951535312, 1.000000000000000000, 0.9510565162951535312, 1.000000000000000000, 0.9510565162951535312, 1.000000000000000000, 0.9510565162951535312, 1.000000000000000000, 0.9510565162951535312, 1.000000000000000000, 0.9510565162951535312, 1.000000000000000000, 0.9510565162951535312, 1.000000000000000000, 0.9510565162951535312, 1.000000000000000000, 0.9510565162951535312, 1.000000000000000000, 0.9510565162951535312, 1.000000000000000000, 0.9510565162951535312, 1.000000000000000000, 0.9510565162951535312, 1.000000000000000000, 0.9510565162951535312, 1.000000000000000000 ) ) 
 REPRESENTATION_ITEM ( '' )  );
#9555 = ORIENTED_EDGE ( 'NONE', *, *, #1362, .F. ) ;
#9556 = VERTEX_POINT ( 'NONE', #10638 ) ;
#9557 = CARTESIAN_POINT ( 'NONE',  ( 6.527192678185836705, 5.883244248022287515, -9.347031149521713219E-14 ) ) ;
#9558 = DIRECTION ( 'NONE',  ( 0.000000000000000000, 1.000000000000000000, 0.000000000000000000 ) ) ;
#9559 = EDGE_CURVE ( 'NONE', #4810, #4189, #2663, .T. ) ;
#9560 = DIRECTION ( 'NONE',  ( -1.000000000000000000, 0.000000000000000000, 0.000000000000000000 ) ) ;
#9561 = PLANE ( 'NONE',  #10418 ) ;
#9562 = CARTESIAN_POINT ( 'NONE',  ( -62.49999999999997158, 45.00000000000001421, 0.000000000000000000 ) ) ;
#9563 = AXIS2_PLACEMENT_3D ( 'NONE', #2972, #12506, #661 ) ;
#9564 = EDGE_CURVE ( 'NONE', #9257, #12356, #10262, .T. ) ;
#9565 = CARTESIAN_POINT ( 'NONE',  ( 53.54508667620428497, 48.29948385550240175, 4.840751629271157874 ) ) ;
#9566 = CARTESIAN_POINT ( 'NONE',  ( 43.34962307344081012, 64.89948385550239607, 2.184720259617164650 ) ) ;
#9567 = CARTESIAN_POINT ( 'NONE',  ( 50.02271294988505446, 48.50051614449765935, -8.000000000000001776 ) ) ;
#9568 = CARTESIAN_POINT ( 'NONE',  ( 5.599999999999999645, 2.020725942163688504, 3.500000000000000000 ) ) ;
#9569 = LINE ( 'NONE', #3275, #10291 ) ;
#9570 = AXIS2_PLACEMENT_3D ( 'NONE', #7560, #2564, #10992 ) ;
#9571 = CARTESIAN_POINT ( 'NONE',  ( 55.94051828345053679, 57.20051614449766930, 4.345558710429044069 ) ) ;
#9572 = CARTESIAN_POINT ( 'NONE',  ( 49.97728705011488870, 57.49948385550241170, -6.000000000000000888 ) ) ;
#9573 = CARTESIAN_POINT ( 'NONE',  ( 8.500000000000000000, -2.886751345948133984, -5.000000000000000000 ) ) ;
#9574 = VERTEX_POINT ( 'NONE', #8367 ) ;
#9575 = CARTESIAN_POINT ( 'NONE',  ( -62.49999999999997158, 32.50000000000001421, -15.00000000000000000 ) ) ;
#9576 = VERTEX_POINT ( 'NONE', #12573 ) ;
#9577 = CARTESIAN_POINT ( 'NONE',  ( 6.533910050139694725, 2.950514251728050485, 5.110440592449069896 ) ) ;
#9578 = DIRECTION ( 'NONE',  ( -1.000000000000000000, 0.000000000000000000, 0.000000000000000000 ) ) ;
#9579 = CYLINDRICAL_SURFACE ( 'NONE', #2450, 2.649999999999985700 ) ;
#9580 = EDGE_CURVE ( 'NONE', #5185, #9272, #5531, .T. ) ;
#9581 = EDGE_CURVE ( 'NONE', #5130, #12476, #5595, .T. ) ;
#9582 = PRESENTATION_STYLE_ASSIGNMENT (( #106 ) ) ;
#9583 = CARTESIAN_POINT ( 'NONE',  ( 52.25172492374522903, 51.59948385550240602, -7.007379884777225953 ) ) ;
#9584 = EDGE_CURVE ( 'NONE', #9377, #4470, #12143, .T. ) ;
#9585 = FACE_OUTER_BOUND ( 'NONE', #1355, .T. ) ;
#9586 = CARTESIAN_POINT ( 'NONE',  ( 46.49166364869456913, 50.30051614449766362, -4.867452303228181343 ) ) ;
#9587 = AXIS2_PLACEMENT_3D ( 'NONE', #12759, #3303, #7526 ) ;
#9588 = CARTESIAN_POINT ( 'NONE',  ( 4.175813232069146785, -2.061359961916366057, 3.570380186727398542 ) ) ;
#9589 = CARTESIAN_POINT ( 'NONE',  ( 45.86712807150323812, 63.29948385550240886, -5.649768623646098220 ) ) ;
#9590 = CARTESIAN_POINT ( 'NONE',  ( -1.959187206999195895E-15, 3.202582148906728765, 1.452965002680430828 ) ) ;
#9591 = CARTESIAN_POINT ( 'NONE',  ( 47.74827507625478518, 58.59948385550238470, 7.007379884777227730 ) ) ;
#9592 = LINE ( 'NONE', #12370, #9354 ) ;
#9593 = ORIENTED_EDGE ( 'NONE', *, *, #343, .F. ) ;
#9594 = ORIENTED_EDGE ( 'NONE', *, *, #2481, .F. ) ;
#9595 = ORIENTED_EDGE ( 'NONE', *, *, #6018, .T. ) ;
#9596 = CARTESIAN_POINT ( 'NONE',  ( 4.142654963991853734, 4.070796997468700162, 1.458723597913840680E-15 ) ) ;
#9597 = CIRCLE ( 'NONE', #12231, 1.500000000000000222 ) ;
#9598 = DIRECTION ( 'NONE',  ( 1.000000000000000000, 0.000000000000000000, 0.000000000000000000 ) ) ;
#9599 = CARTESIAN_POINT ( 'NONE',  ( -4.000000000000000000, 2.309401076758498483, -0.4999999999999927280 ) ) ;
#9600 = FACE_OUTER_BOUND ( 'NONE', #3419, .T. ) ;
#9601 = CARTESIAN_POINT ( 'NONE',  ( 45.90387839640214196, 54.69948385550240744, 5.676469297603166098 ) ) ;
#9602 = AXIS2_PLACEMENT_3D ( 'NONE', #11091, #9023, #9168 ) ;
#9603 = CARTESIAN_POINT ( 'NONE',  ( 56.65037692655921120, 47.10051614449766078, 2.184720259617097593 ) ) ;
#9604 = CARTESIAN_POINT ( 'NONE',  ( 4.000000000000001776, 0.000000000000000000, -2.200000000000001066 ) ) ;
#9605 = VECTOR ( 'NONE', #2253, 1000.000000000000000 ) ;
#9606 = CARTESIAN_POINT ( 'NONE',  ( 49.97728705011488159, 45.49948385550240459, -7.000000000000000888 ) ) ;
#9607 = VECTOR ( 'NONE', #1224, 1000.000000000000000 ) ;
#9608 = EDGE_CURVE ( 'NONE', #12388, #6557, #2393, .T. ) ;
#9609 = CARTESIAN_POINT ( 'NONE',  ( 58.41169779390614281, 53.99948385550241170, -0.02388180880523160798 ) ) ;
#9610 = EDGE_LOOP ( 'NONE', ( #4921, #11039, #3060, #9325 ) ) ;
#9611 = VERTEX_POINT ( 'NONE', #10706 ) ;
#9612 = DIRECTION ( 'NONE',  ( -1.000000000000000000, 0.000000000000000000, 0.000000000000000000 ) ) ;
#9613 = CARTESIAN_POINT ( 'NONE',  ( 6.534838248920900483, -5.903531555104836848, 4.671345613696493211E-16 ) ) ;
#9614 = CIRCLE ( 'NONE', #6719, 5.000000000000000888 ) ;
#9615 = CARTESIAN_POINT ( 'NONE',  ( 51.92680522751238925, 45.40051614449765793, 6.007379884777208190 ) ) ;
#9616 = CARTESIAN_POINT ( 'NONE',  ( 57.36023556966787851, 57.00051614449766646, 0.02388180880515038476 ) ) ;
#9617 = CARTESIAN_POINT ( 'NONE',  ( 57.60143344285433642, 47.89948385550240317, -2.493737253992118319 ) ) ;
#9618 = DIRECTION ( 'NONE',  ( 0.000000000000000000, -0.8660254037844380415, -0.5000000000000009992 ) ) ;
#9619 = CARTESIAN_POINT ( 'NONE',  ( 45.31609314410960820, 56.30051614449766362, -6.485486291978072693 ) ) ;
#9620 = ADVANCED_FACE ( 'NONE', ( #7531 ), #3753, .T. ) ;
#9621 = VERTEX_POINT ( 'NONE', #8770 ) ;
#9622 = VERTEX_POINT ( 'NONE', #8632 ) ;
#9623 = ORIENTED_EDGE ( 'NONE', *, *, #8471, .F. ) ;
#9624 = EDGE_LOOP ( 'NONE', ( #13636, #12496, #6190, #179 ) ) ;
#9625 = CARTESIAN_POINT ( 'NONE',  ( -12.99038105676654453, -27.50000000000006040, -9.000000000000000000 ) ) ;
#9626 = DIRECTION ( 'NONE',  ( 0.000000000000000000, 0.000000000000000000, 1.000000000000000000 ) ) ;
#9627 = CARTESIAN_POINT ( 'NONE',  ( 13.99999999999999822, 0.000000000000000000, 1.610000000000000098 ) ) ;
#9628 = LINE ( 'NONE', #10861, #3609 ) ;
#9629 = ADVANCED_BREP_SHAPE_REPRESENTATION ( '', ( #1187, #430 ), #3078 ) ;
#9630 = CARTESIAN_POINT ( 'NONE',  ( 46.45491332379572924, 49.29948385550240886, -4.840751629271157874 ) ) ;
#9631 = CARTESIAN_POINT ( 'NONE',  ( -62.49999999999997158, 32.50000000000001421, 15.00000000000000000 ) ) ;
#9632 = CARTESIAN_POINT ( 'NONE',  ( 57.61547081786810764, 46.90051614449766504, -2.450534656007114176 ) ) ;
#9633 = AXIS2_PLACEMENT_3D ( 'NONE', #7014, #9978, #498 ) ;
#9634 = CARTESIAN_POINT ( 'NONE',  ( -62.49999999999997158, 32.50000000000001421, 9.999999999999998224 ) ) ;
#9635 = CARTESIAN_POINT ( 'NONE',  ( 7.900000000000002132, 0.000000000000000000, 7.900000000000002132 ) ) ;
#9636 =( BOUNDED_SURFACE ( )  B_SPLINE_SURFACE ( 3, 2, ( 
 ( #3575, #11935, #2454 ),
 ( #12074, #11025, #7728 ),
 ( #444, #12140, #1409 ),
 ( #5656, #10127, #8903 ),
 ( #6962, #9990, #2662 ),
 ( #11167, #6890, #4612 ) ),
 .UNSPECIFIED., .F., .F., .F. ) 
 B_SPLINE_SURFACE_WITH_KNOTS ( ( 4, 2, 4 ),
 ( 3, 3 ),
 ( 0.02032853247518126918, 0.02278863295364821906, 0.02524873343211517240 ),
 ( 0.000000000000000000, 1.000000000000000000 ),
 .UNSPECIFIED. ) 
 GEOMETRIC_REPRESENTATION_ITEM ( )  RATIONAL_B_SPLINE_SURFACE ( (
 ( 1.000000000000000000, 0.8047781615896837382, 1.000000000000000000),
 ( 1.000000000000000000, 0.8123767586289252218, 1.000000000000000000),
 ( 1.000000000000000000, 0.8190662415564388121, 1.000000000000000000),
 ( 1.000000000000000000, 0.8192361015669026303, 1.000000000000000000),
 ( 1.000000000000000000, 0.8126135807103900266, 1.000000000000000000),
 ( 1.000000000000000000, 0.8047712338318593339, 1.000000000000000000) ) ) 
 REPRESENTATION_ITEM ( '' )  SURFACE ( )  );
#9637 = CARTESIAN_POINT ( 'NONE',  ( 50.02271294988505446, 60.50051614449765935, -7.000000000000000888 ) ) ;
#9638 = CARTESIAN_POINT ( 'NONE',  ( 48.07319477248768180, 60.59948385550240602, 6.007379884777225953 ) ) ;
#9639 = ORIENTED_EDGE ( 'NONE', *, *, #10310, .F. ) ;
#9640 = CARTESIAN_POINT ( 'NONE',  ( 3.260336594487419859, -23.79080536174652494, -8.999999999999998224 ) ) ;
#9641 = ORIENTED_EDGE ( 'NONE', *, *, #267, .T. ) ;
#9642 = CYLINDRICAL_SURFACE ( 'NONE', #404, 5.000000000000000000 ) ;
#9643 = EDGE_CURVE ( 'NONE', #5822, #13042, #218, .T. ) ;
#9644 = DIRECTION ( 'NONE',  ( -0.000000000000000000, -0.000000000000000000, 1.000000000000000000 ) ) ;
#9645 = CARTESIAN_POINT ( 'NONE',  ( 0.000000000000000000, 0.000000000000000000, 0.000000000000000000 ) ) ;
#9646 = CARTESIAN_POINT ( 'NONE',  ( 52.29715082351547295, 48.39948385550240317, 6.992620115222774047 ) ) ;
#9647 = DIRECTION ( 'NONE',  ( -0.000000000000000000, -0.000000000000000000, -1.000000000000000000 ) ) ;
#9648 = CARTESIAN_POINT ( 'NONE',  ( 55.71335778527780036, 48.90051614449766504, -1.832500667257213056 ) ) ;
#9649 = EDGE_CURVE ( 'NONE', #11305, #6619, #3971, .T. ) ;
#9650 = CARTESIAN_POINT ( 'NONE',  ( 0.000000000000000000, 0.000000000000000000, 2.500000000000000444 ) ) ;
#9651 = DIRECTION ( 'NONE',  ( -0.9768494444668812671, -0.2139279384389642935, 0.000000000000000000 ) ) ;
#9652 = CARTESIAN_POINT ( 'NONE',  ( 6.534224484704327374, -5.901860969583205829, 2.643887195172161483E-14 ) ) ;
#9653 = CARTESIAN_POINT ( 'NONE',  ( 56.65037692655918988, 59.89948385550241028, -2.184720259617163762 ) ) ;
#9654 = CARTESIAN_POINT ( 'NONE',  ( 2.449293598294706513E-15, -20.00000000000000000, 9.000000000000000000 ) ) ;
#9655 = VERTEX_POINT ( 'NONE', #2258 ) ;
#9656 = EDGE_CURVE ( 'NONE', #3637, #2102, #6843, .T. ) ;
#9657 = ADVANCED_FACE ( 'NONE', ( #7737 ), #9739, .T. ) ;
#9658 = UNCERTAINTY_MEASURE_WITH_UNIT (LENGTH_MEASURE( 1.000000000000000082E-05 ), #5035, 'distance_accuracy_value', 'NONE');
#9659 = ORIENTED_EDGE ( 'NONE', *, *, #2861, .F. ) ;
#9660 = ORIENTED_EDGE ( 'NONE', *, *, #9047, .T. ) ;
#9661 = FACE_BOUND ( 'NONE', #12305, .T. ) ;
#9662 = DIRECTION ( 'NONE',  ( 1.000000000000000000, 0.000000000000000000, 0.000000000000000000 ) ) ;
#9663 = CARTESIAN_POINT ( 'NONE',  ( 4.086376042167606748, -1.979461949354202499, 3.571471332069183990 ) ) ;
#9664 = ADVANCED_FACE ( 'NONE', ( #190 ), #6763, .T. ) ;
#9665 = CARTESIAN_POINT ( 'NONE',  ( 4.799999999999999822, 0.000000000000000000, -1.000000000000000000 ) ) ;
#9666 = CARTESIAN_POINT ( 'NONE',  ( 52.25172492374522903, 55.59948385550241312, -7.007379884777227730 ) ) ;
#9667 = CARTESIAN_POINT ( 'NONE',  ( 44.05948171654945611, 56.20051614449764799, -4.345558710429044069 ) ) ;
#9668 = DIRECTION ( 'NONE',  ( -0.9768494444668812671, -0.2139279384389642935, 0.000000000000000000 ) ) ;
#9669 = CARTESIAN_POINT ( 'NONE',  ( 43.18075615816989199, 63.19948385550240744, -4.924951120819313743 ) ) ;
#9670 = PRESENTATION_STYLE_ASSIGNMENT (( #1076 ) ) ;
#9671 = CARTESIAN_POINT ( 'NONE',  ( 45.31609314410967926, 56.69948385550240744, 6.485486291978119766 ) ) ;
#9672 = B_SPLINE_CURVE_WITH_KNOTS ( 'NONE', 3,
 ( #3229, #5248, #2046, #4132, #43 ),
 .UNSPECIFIED., .F., .F.,
 ( 4, 1, 4 ),
 ( 9.359404341228126911E-20, 0.002886751345948132021, 0.005773502691896264041 ),
 .UNSPECIFIED. ) ;
#9673 = VERTEX_POINT ( 'NONE', #4414 ) ;
#9674 = ORIENTED_EDGE ( 'NONE', *, *, #8230, .F. ) ;
#9675 = DIRECTION ( 'NONE',  ( 1.000000000000000000, 0.000000000000000000, 0.000000000000000000 ) ) ;
#9676 = CIRCLE ( 'NONE', #8358, 0.7499999999999997780 ) ;
#9677 = CYLINDRICAL_SURFACE ( 'NONE', #2214, 5.000000000000007994 ) ;
#9678 = CARTESIAN_POINT ( 'NONE',  ( 46.49166364869456913, 46.30051614449766362, -4.867452303228181343 ) ) ;
#9679 = CARTESIAN_POINT ( 'NONE',  ( 1.000000000000000444, -15.10102051443364246, -8.999999999999998224 ) ) ;
#9680 = CARTESIAN_POINT ( 'NONE',  ( 42.39856655714566358, 48.89948385550241028, 2.493737253992119207 ) ) ;
#9681 = CARTESIAN_POINT ( 'NONE',  ( -1.250000000000000000, -6.429618962271402616, -1.000000000000000000 ) ) ;
#9682 = CARTESIAN_POINT ( 'NONE',  ( 52.62207051974829852, 54.60051614449766788, -7.992620115222797139 ) ) ;
#9683 = AXIS2_PLACEMENT_3D ( 'NONE', #1756, #3015, #11381 ) ;
#9684 = ADVANCED_FACE ( 'NONE', ( #11871 ), #9804, .T. ) ;
#9685 = EDGE_LOOP ( 'NONE', ( #13244, #7423, #7485, #2506, #4588 ) ) ;
#9686 = AXIS2_PLACEMENT_3D ( 'NONE', #6984, #1711, #660 ) ;
#9687 = EDGE_LOOP ( 'NONE', ( #738, #13639, #13591, #5077 ) ) ;
#9688 = VERTEX_POINT ( 'NONE', #8838 ) ;
#9689 = ORIENTED_EDGE ( 'NONE', *, *, #7806, .F. ) ;
#9690 = CARTESIAN_POINT ( 'NONE',  ( 2.500000000000000444, 0.000000000000000000, -25.03750572909317285 ) ) ;
#9691 =( NAMED_UNIT ( * ) PLANE_ANGLE_UNIT ( ) SI_UNIT ( $, .RADIAN. ) );
#9692 = DIRECTION ( 'NONE',  ( -0.7071067811865530128, 0.000000000000000000, 0.7071067811865421326 ) ) ;
#9693 = CARTESIAN_POINT ( 'NONE',  ( 7.900000000000002132, 0.000000000000000000, 0.000000000000000000 ) ) ;
#9694 =( GEOMETRIC_REPRESENTATION_CONTEXT ( 3 ) GLOBAL_UNCERTAINTY_ASSIGNED_CONTEXT ( ( #9658 ) ) GLOBAL_UNIT_ASSIGNED_CONTEXT ( ( #5035, #13581, #12344 ) ) REPRESENTATION_CONTEXT ( 'NONE', 'WORKASPACE' ) );
#9695 =( NAMED_UNIT ( * ) SI_UNIT ( $, .STERADIAN. ) SOLID_ANGLE_UNIT ( ) );
#9696 = CARTESIAN_POINT ( 'NONE',  ( 51.97223112728254790, 52.39948385550241028, 5.992620115222778487 ) ) ;
#9697 = AXIS2_PLACEMENT_3D ( 'NONE', #710, #6217, #11235 ) ;
#9698 = CARTESIAN_POINT ( 'NONE',  ( 42.63976443033212149, 62.99948385550241170, 0.02388180880522514787 ) ) ;
#9699 = CARTESIAN_POINT ( 'NONE',  ( 41.58830220609386430, 46.00051614449764514, -0.02388180880514929535 ) ) ;
#9700 = CIRCLE ( 'NONE', #3737, 12.49999999999999645 ) ;
#9701 = LINE ( 'NONE', #225, #6251 ) ;
#9702 = CARTESIAN_POINT ( 'NONE',  ( 0.000000000000000000, 0.000000000000000000, 3.299999999999999822 ) ) ;
#9703 = CARTESIAN_POINT ( 'NONE',  ( 47.74827507625469281, 60.40051614449767214, -7.007379884777203749 ) ) ;
#9704 = CARTESIAN_POINT ( 'NONE',  ( 55.08986747509847248, 57.79948385550240175, -3.727524721679197572 ) ) ;
#9705 = VERTEX_POINT ( 'NONE', #12834 ) ;
#9706 = AXIS2_PLACEMENT_3D ( 'NONE', #6730, #3615, #5833 ) ;
#9707 = DIRECTION ( 'NONE',  ( -1.000000000000000000, 0.000000000000000000, 0.000000000000000000 ) ) ;
#9708 = ORIENTED_EDGE ( 'NONE', *, *, #7466, .T. ) ;
#9709 = PLANE ( 'NONE',  #4619 ) ;
#9710 = MECHANICAL_DESIGN_GEOMETRIC_PRESENTATION_REPRESENTATION (  '', ( #5975 ), #13532 ) ;
#9711 = CARTESIAN_POINT ( 'NONE',  ( 62.49999999999998579, 45.00000000000001421, 5.000000000000000000 ) ) ;
#9712 = ADVANCED_FACE ( 'NONE', ( #8564 ), #12901, .F. ) ;
#9713 = CARTESIAN_POINT ( 'NONE',  ( 6.323290364500451233, 2.010128762267162639, 4.999999999999998224 ) ) ;
#9714 = CARTESIAN_POINT ( 'NONE',  ( 54.09612160359786515, 49.69948385550240744, -5.676469297603166098 ) ) ;
#9715 =( BOUNDED_SURFACE ( )  B_SPLINE_SURFACE ( 3, 2, ( 
 ( #2810, #5928, #13368 ),
 ( #2876, #637, #926 ),
 ( #8138, #5176, #1685 ),
 ( #12484, #4889, #9104 ),
 ( #4963, #9383, #7998 ),
 ( #3775, #12412, #7099 ) ),
 .UNSPECIFIED., .F., .F., .F. ) 
 B_SPLINE_SURFACE_WITH_KNOTS ( ( 4, 2, 4 ),
 ( 3, 3 ),
 ( 0.02367865728600892020, 0.02663179453327098323, 0.02958493178053304279 ),
 ( 0.000000000000000000, 1.000000000000000000 ),
 .UNSPECIFIED. ) 
 GEOMETRIC_REPRESENTATION_ITEM ( )  RATIONAL_B_SPLINE_SURFACE ( (
 ( 1.000000000000000000, 0.8047781103519402457, 1.000000000000000000),
 ( 1.000000000000000000, 0.8123785825973208752, 1.000000000000000000),
 ( 1.000000000000000000, 0.8190671539297160741, 1.000000000000000000),
 ( 1.000000000000000000, 0.8192352255325974220, 1.000000000000000000),
 ( 1.000000000000000000, 0.8126129676842754890, 1.000000000000000000),
 ( 1.000000000000000000, 0.8047712537969723412, 1.000000000000000000) ) ) 
 REPRESENTATION_ITEM ( '' )  SURFACE ( )  );
#9716 = VECTOR ( 'NONE', #4281, 1000.000000000000000 ) ;
#9717 = FACE_OUTER_BOUND ( 'NONE', #8523, .T. ) ;
#9718 = CARTESIAN_POINT ( 'NONE',  ( 49.97728705011494554, 59.50051614449765935, 6.000000000000000888 ) ) ;
#9719 = EDGE_CURVE ( 'NONE', #11951, #10162, #5662, .T. ) ;
#9720 = DIRECTION ( 'NONE',  ( 9.710251638871371392E-17, 5.969973981896233748E-17, 1.000000000000000000 ) ) ;
#9721 = DIRECTION ( 'NONE',  ( 0.000000000000000000, 0.000000000000000000, 1.000000000000000000 ) ) ;
#9722 =( NAMED_UNIT ( * ) PLANE_ANGLE_UNIT ( ) SI_UNIT ( $, .RADIAN. ) );
#9723 = CARTESIAN_POINT ( 'NONE',  ( 56.66441430157296821, 62.09948385550239891, 2.141517661632100111 ) ) ;
#9724 = CARTESIAN_POINT ( 'NONE',  ( 0.1983443223721600701, -5.300482436767282479, -0.8192951148925879945 ) ) ;
#9725 = B_SPLINE_CURVE_WITH_KNOTS ( 'NONE', 3,
 ( #9799, #5725, #9031, #11936 ),
 .UNSPECIFIED., .F., .F.,
 ( 4, 4 ),
 ( 0.002080789711329296236, 0.004173039763574516031 ),
 .UNSPECIFIED. ) ;
#9726 = VERTEX_POINT ( 'NONE', #3377 ) ;
#9727 = APPLICATION_CONTEXT ( 'automotive_design' ) ;
#9728 = EDGE_LOOP ( 'NONE', ( #6724, #11569, #5237, #6920 ) ) ;
#9729 = CARTESIAN_POINT ( 'NONE',  ( 4.158413352280809328, 4.089743253945647972, 1.634918261399485461E-15 ) ) ;
#9730 = CONICAL_SURFACE ( 'NONE', #2651, 2.059999999999998721, 0.9599310885968738161 ) ;
#9731 = EDGE_CURVE ( 'NONE', #13327, #1558, #10809, .T. ) ;
#9732 = CARTESIAN_POINT ( 'NONE',  ( 25.00000000000000711, -20.00000000000000000, -20.00000000000000000 ) ) ;
#9733 = CARTESIAN_POINT ( 'NONE',  ( 0.000000000000000000, 0.000000000000000000, -4.694516984716113228 ) ) ;
#9734 = DIRECTION ( 'NONE',  ( -0.000000000000000000, -0.000000000000000000, -1.000000000000000000 ) ) ;
#9735 = ADVANCED_FACE ( 'NONE', ( #11806, #5731 ), #3581, .T. ) ;
#9736 = CARTESIAN_POINT ( 'NONE',  ( 55.94051828345050836, 53.79948385550240175, -4.345558710429103577 ) ) ;
#9737 = CARTESIAN_POINT ( 'NONE',  ( 44.03140696652198471, 51.80051614449766362, 4.306917132069485454 ) ) ;
#9738 = EDGE_CURVE ( 'NONE', #4029, #11042, #10578, .T. ) ;
#9739 = CYLINDRICAL_SURFACE ( 'NONE', #2197, 12.49999999999999645 ) ;
#9740 = CARTESIAN_POINT ( 'NONE',  ( 49.97728705011488159, 49.49948385550240459, -7.000000000000000888 ) ) ;
#9741 = PRESENTATION_STYLE_ASSIGNMENT (( #12838 ) ) ;
#9742 = CONICAL_SURFACE ( 'NONE', #1079, 5.000000000000000000, 1.047197551196600296 ) ;
#9743 = CARTESIAN_POINT ( 'NONE',  ( 56.79116909180255135, 59.79948385550240175, -4.963592699179005585 ) ) ;
#9744 = EDGE_LOOP ( 'NONE', ( #8745, #6362, #8959, #6052 ) ) ;
#9745 = ORIENTED_EDGE ( 'NONE', *, *, #3430, .F. ) ;
#9746 = DIRECTION ( 'NONE',  ( 0.000000000000000000, 0.000000000000000000, -1.000000000000000000 ) ) ;
#9747 = AXIS2_PLACEMENT_3D ( 'NONE', #2739, #2595, #13032 ) ;
#9748 = DIRECTION ( 'NONE',  ( -0.000000000000000000, -0.000000000000000000, 1.000000000000000000 ) ) ;
#9749 = CARTESIAN_POINT ( 'NONE',  ( 55.11794222512599362, 54.80051614449764941, -3.688883143319583446 ) ) ;
#9750 = CARTESIAN_POINT ( 'NONE',  ( 1.567478505476134606E-15, 4.618802153517012066, -3.433295621305382905 ) ) ;
#9751 = CARTESIAN_POINT ( 'NONE',  ( 43.20883090819745576, 50.79948385550240175, 4.963592699179006473 ) ) ;
#9752 = CARTESIAN_POINT ( 'NONE',  ( 54.09612160359786515, 55.69948385550240744, -5.676469297603166098 ) ) ;
#9753 = CARTESIAN_POINT ( 'NONE',  ( 3.878096787214571517, 3.381939201670116191, 1.142309474598433461 ) ) ;
#9754 = CARTESIAN_POINT ( 'NONE',  ( 45.31609314410960820, 58.30051614449765651, -6.485486291978072693 ) ) ;
#9755 = AXIS2_PLACEMENT_3D ( 'NONE', #2718, #13209, #2931 ) ;
#9756 = VECTOR ( 'NONE', #11922, 1000.000000000000000 ) ;
#9757 = ORIENTED_EDGE ( 'NONE', *, *, #11921, .T. ) ;
#9758 = ORIENTED_EDGE ( 'NONE', *, *, #11753, .F. ) ;
#9759 = EDGE_LOOP ( 'NONE', ( #7059, #4943, #12289, #10090 ) ) ;
#9760 = ORIENTED_EDGE ( 'NONE', *, *, #11225, .T. ) ;
#9761 = DIRECTION ( 'NONE',  ( 0.000000000000000000, 0.000000000000000000, 1.000000000000000000 ) ) ;
#9762 = SURFACE_STYLE_FILL_AREA ( #9831 ) ;
#9763 = DIRECTION ( 'NONE',  ( -0.000000000000000000, 0.000000000000000000, -1.000000000000000000 ) ) ;
#9764 = ADVANCED_FACE ( 'NONE', ( #642 ), #4893, .T. ) ;
#9765 = DIRECTION ( 'NONE',  ( -0.000000000000000000, -0.000000000000000000, -1.000000000000000000 ) ) ;
#9766 = CARTESIAN_POINT ( 'NONE',  ( 51.92680522751233951, 59.59948385550240602, -6.007379884777223289 ) ) ;
#9767 = CARTESIAN_POINT ( 'NONE',  ( 45.86712807150329496, 45.70051614449766220, 5.649768623646139964 ) ) ;
#9768 = CARTESIAN_POINT ( 'NONE',  ( 58.41169779390614281, 45.00051614449765225, 0.02388180880515032231 ) ) ;
#9769 = CARTESIAN_POINT ( 'NONE',  ( 20.00000000000000000, -20.00000000000000000, -23.00000000000000000 ) ) ;
#9770 = CARTESIAN_POINT ( 'NONE',  ( 0.4465819873852039379, 5.773502691896261751, 3.331019006688249527E-17 ) ) ;
#9771 = CARTESIAN_POINT ( 'NONE',  ( 43.34962307344078880, 58.10051614449766078, -2.184720259617096705 ) ) ;
#9772 = CARTESIAN_POINT ( 'NONE',  ( 44.30067958973596376, 62.89948385550240317, 1.875703265242204099 ) ) ;
#9773 = B_SPLINE_CURVE_WITH_KNOTS ( 'NONE', 3,
 ( #9195, #4771, #10011, #528, #13389, #9265 ),
 .UNSPECIFIED., .F., .F.,
 ( 4, 2, 4 ),
 ( 0.002452478801916376308, 0.003676905084148007850, 0.004901331366379639391 ),
 .UNSPECIFIED. ) ;
#9774 = ORIENTED_EDGE ( 'NONE', *, *, #2973, .F. ) ;
#9775 = CARTESIAN_POINT ( 'NONE',  ( -20.00000000000000000, -25.00000000000000000, -23.00000000000000000 ) ) ;
#9776 = ORIENTED_EDGE ( 'NONE', *, *, #5011, .F. ) ;
#9777 = CARTESIAN_POINT ( 'NONE',  ( 3.020236159542450949, -23.98474259401938014, 15.00000000000000355 ) ) ;
#9778 = AXIS2_PLACEMENT_3D ( 'NONE', #2342, #6580, #4 ) ;
#9779 = CARTESIAN_POINT ( 'NONE',  ( 75.00000000000001421, -4.999999999999974243, 6.123233995736766282E-16 ) ) ;
#9780 = CARTESIAN_POINT ( 'NONE',  ( 4.086376042167608524, -4.082715877136868343, 0.07147133206917789805 ) ) ;
#9781 = CARTESIAN_POINT ( 'NONE',  ( 42.63976443033212860, 54.99948385550241170, 0.02388180880522514787 ) ) ;
#9782 = VECTOR ( 'NONE', #409, 1000.000000000000000 ) ;
#9783 = CYLINDRICAL_SURFACE ( 'NONE', #6430, 5.000000000000007994 ) ;
#9784 = CARTESIAN_POINT ( 'NONE',  ( 44.28664221472221385, 57.90051614449765793, 1.832500667257213722 ) ) ;
#9785 = CARTESIAN_POINT ( 'NONE',  ( 5.599999999999998757, 0.000000000000000000, 0.000000000000000000 ) ) ;
#9786 = CARTESIAN_POINT ( 'NONE',  ( 0.9183817310753816798, -24.91493387504114665, 15.00000000000000355 ) ) ;
#9787 = CARTESIAN_POINT ( 'NONE',  ( 6.403457969954083673, -5.776886471390910494, 4.740078563816561288E-16 ) ) ;
#9788 = CARTESIAN_POINT ( 'NONE',  ( 54.13287192849676188, 64.29948385550241596, 5.649768623646098220 ) ) ;
#9789 = CARTESIAN_POINT ( 'NONE',  ( 0.01055556052339245120, -4.575665857285984295, -2.074714256722479888 ) ) ;
#9790 = EDGE_LOOP ( 'NONE', ( #4485, #4609, #4764, #330, #1358 ) ) ;
#9791 = ORIENTED_EDGE ( 'NONE', *, *, #6610, .F. ) ;
#9792 = EDGE_CURVE ( 'NONE', #6392, #10628, #575, .T. ) ;
#9793 = UNCERTAINTY_MEASURE_WITH_UNIT (LENGTH_MEASURE( 1.000000000000000082E-05 ), #8209, 'distance_accuracy_value', 'NONE');
#9794 = EDGE_LOOP ( 'NONE', ( #9408, #5669, #8625, #11162, #7618, #4256, #2415, #1232 ) ) ;
#9795 = CARTESIAN_POINT ( 'NONE',  ( -7.500000000000013323, -7.009618943233427935, -9.000000000000000000 ) ) ;
#9796 = ADVANCED_FACE ( 'NONE', ( #2670 ), #11104, .F. ) ;
#9797 = CARTESIAN_POINT ( 'NONE',  ( 0.4465819873851989974, -2.886751345948120218, 4.999999999999999112 ) ) ;
#9798 =( BOUNDED_SURFACE ( )  B_SPLINE_SURFACE ( 3, 2, ( 
 ( #8697, #2323, #8430 ),
 ( #7397, #184, #55 ),
 ( #12760, #11608, #6432 ),
 ( #2120, #2252, #6501 ),
 ( #5461, #1070, #5322 ),
 ( #9663, #7927, #4544 ) ),
 .UNSPECIFIED., .F., .F., .F. ) 
 B_SPLINE_SURFACE_WITH_KNOTS ( ( 4, 2, 4 ),
 ( 3, 3 ),
 ( 0.01651999345535504551, 0.01858032176739835006, 0.02064065007944165114 ),
 ( 0.000000000000000000, 1.000000000000000000 ),
 .UNSPECIFIED. ) 
 GEOMETRIC_REPRESENTATION_ITEM ( )  RATIONAL_B_SPLINE_SURFACE ( (
 ( 1.000000000000000000, 0.8047781103519391355, 1.000000000000000000),
 ( 1.000000000000000000, 0.8123785825613523137, 1.000000000000000000),
 ( 1.000000000000000000, 0.8190671539776074317, 1.000000000000000000),
 ( 1.000000000000000000, 0.8192352254847047321, 1.000000000000000000),
 ( 1.000000000000000000, 0.8126129677202470480, 1.000000000000000000),
 ( 1.000000000000000000, 0.8047712537969722302, 1.000000000000000000) ) ) 
 REPRESENTATION_ITEM ( '' )  SURFACE ( )  );
#9799 = CARTESIAN_POINT ( 'NONE',  ( 3.973110223767137850, -2.261493176400255405E-11, -3.565797985667433334 ) ) ;
#9800 = DIRECTION ( 'NONE',  ( 0.000000000000000000, 0.000000000000000000, -1.000000000000000000 ) ) ;
#9801 = DIRECTION ( 'NONE',  ( 1.000000000000000000, 3.469446951953615668E-16, -0.000000000000000000 ) ) ;
#9802 = CARTESIAN_POINT ( 'NONE',  ( 52.29715082351547295, 54.39948385550239607, 6.992620115222774047 ) ) ;
#9803 = CARTESIAN_POINT ( 'NONE',  ( 50.02271294988505446, 52.50051614449765935, -7.000000000000000888 ) ) ;
#9804 = PLANE ( 'NONE',  #7309 ) ;
#9805 = CARTESIAN_POINT ( 'NONE',  ( 47.74827507625478518, 54.59948385550239180, 7.007379884777227730 ) ) ;
#9806 = CARTESIAN_POINT ( 'NONE',  ( 45.27934281921075410, 61.29948385550240886, -6.458785618021043895 ) ) ;
#9807 = CIRCLE ( 'NONE', #8935, 15.00000000000000000 ) ;
#9808 = ORIENTED_EDGE ( 'NONE', *, *, #4262, .F. ) ;
#9809 = VERTEX_POINT ( 'NONE', #9178 ) ;
#9810 = ORIENTED_EDGE ( 'NONE', *, *, #5683, .T. ) ;
#9811 = FACE_OUTER_BOUND ( 'NONE', #8147, .T. ) ;
#9812 = VECTOR ( 'NONE', #3972, 1000.000000000000000 ) ;
#9813 = AXIS2_PLACEMENT_3D ( 'NONE', #2189, #4476, #3306 ) ;
#9814 = EDGE_CURVE ( 'NONE', #1099, #11408, #9054, .T. ) ;
#9815 = CARTESIAN_POINT ( 'NONE',  ( -1.935715396507168721E-15, 2.686816014504566752, 2.346298152288372130 ) ) ;
#9816 = CARTESIAN_POINT ( 'NONE',  ( 55.71335778527780036, 52.90051614449766504, -1.832500667257213056 ) ) ;
#9817 = CARTESIAN_POINT ( 'NONE',  ( 44.03140696652198471, 63.80051614449764941, 4.306917132069485454 ) ) ;
#9818 = AXIS2_PLACEMENT_3D ( 'NONE', #12568, #6161, #10358 ) ;
#9819 = CARTESIAN_POINT ( 'NONE',  ( 52.62207051974839089, 54.39948385550241028, 7.992620115222770494 ) ) ;
#9820 = CARTESIAN_POINT ( 'NONE',  ( 54.13287192849676188, 58.29948385550240175, 5.649768623646098220 ) ) ;
#9821 = CARTESIAN_POINT ( 'NONE',  ( -4.000000000000000000, -2.309401076758515803, -0.4999999999999995559 ) ) ;
#9822 = VECTOR ( 'NONE', #11454, 1000.000000000000000 ) ;
#9823 = CARTESIAN_POINT ( 'NONE',  ( 57.60143344285435774, 63.10051614449766078, 2.493737253992045044 ) ) ;
#9824 = VERTEX_POINT ( 'NONE', #6969 ) ;
#9825 = EDGE_CURVE ( 'NONE', #4959, #7079, #8075, .T. ) ;
#9826 = ORIENTED_EDGE ( 'NONE', *, *, #11002, .T. ) ;
#9827 = EDGE_CURVE ( 'NONE', #7673, #7674, #10207, .T. ) ;
#9828 = ORIENTED_EDGE ( 'NONE', *, *, #10636, .F. ) ;
#9829 = ORIENTED_EDGE ( 'NONE', *, *, #11221, .T. ) ;
#9830 = DIRECTION ( 'NONE',  ( 0.000000000000000000, 0.000000000000000000, 1.000000000000000000 ) ) ;
#9831 = FILL_AREA_STYLE ('',( #8733 ) ) ;
#9832 = CARTESIAN_POINT ( 'NONE',  ( 0.3117969352650131198, 2.419842229202155970, 4.999999999999999112 ) ) ;
#9833 = FACE_OUTER_BOUND ( 'NONE', #3840, .T. ) ;
#9834 = CARTESIAN_POINT ( 'NONE',  ( 49.97728705011488870, 59.49948385550240459, -6.000000000000000888 ) ) ;
#9835 = CARTESIAN_POINT ( 'NONE',  ( 57.36023556966787851, 49.00051614449764514, 0.02388180880515038476 ) ) ;
#9836 = CARTESIAN_POINT ( 'NONE',  ( 42.38452918213190657, 51.90051614449765793, 2.450534656007115508 ) ) ;
#9837 = PLANE ( 'NONE',  #6674 ) ;
#9838 = DIRECTION ( 'NONE',  ( 0.000000000000000000, 0.4999999999999991118, -0.8660254037844390407 ) ) ;
#9839 = CARTESIAN_POINT ( 'NONE',  ( 44.03140696652198471, 61.80051614449767072, 4.306917132069485454 ) ) ;
#9840 = ORIENTED_EDGE ( 'NONE', *, *, #13414, .T. ) ;
#9841 = ADVANCED_FACE ( 'NONE', ( #12281 ), #2743, .F. ) ;
#9842 = CARTESIAN_POINT ( 'NONE',  ( -65.14999999999996305, 32.50000000000001421, -10.00000000000000178 ) ) ;
#9843 = ORIENTED_EDGE ( 'NONE', *, *, #13608, .T. ) ;
#9844 = DIRECTION ( 'NONE',  ( 1.000000000000000000, 0.000000000000000000, 0.000000000000000000 ) ) ;
#9845 = CARTESIAN_POINT ( 'NONE',  ( 2.449293598294706513E-15, -35.00000000000000000, -9.000000000000000000 ) ) ;
#9846 = FACE_OUTER_BOUND ( 'NONE', #10869, .T. ) ;
#9847 = CARTESIAN_POINT ( 'NONE',  ( 50.00000000000000000, 74.50000000000002842, 0.000000000000000000 ) ) ;
#9848 = CARTESIAN_POINT ( 'NONE',  ( 44.03140696652192787, 59.19948385550238612, -4.306917132069425058 ) ) ;
#9849 = AXIS2_PLACEMENT_3D ( 'NONE', #9575, #8474, #7441 ) ;
#9850 = B_SPLINE_CURVE_WITH_KNOTS ( 'NONE', 3,
 ( #4342, #12892, #10698, #11731, #2321, #6498, #4471, #9596, #13657, #9729, #1212, #6558, #1142, #4205, #8428, #10493 ),
 .UNSPECIFIED., .F., .F.,
 ( 4, 3, 3, 3, 3, 4 ),
 ( 0.000000000000000000, 3.315506744709155554E-05, 6.608280158698769959E-05, 0.0001026520855291340739, 0.0001376952025664813454, 0.0001398064759190616429 ),
 .UNSPECIFIED. ) ;
#9851 = CARTESIAN_POINT ( 'NONE',  ( 56.30877334542961421, 57.00051614449766646, 0.02388180880515774693 ) ) ;
#9852 = DIRECTION ( 'NONE',  ( -0.7779254092217071648, -0.6283566325640553840, 0.000000000000000000 ) ) ;
#9853 = CARTESIAN_POINT ( 'NONE',  ( 4.000000000000000000, 2.309401076758515803, -0.4999999999999995559 ) ) ;
#9854 = CARTESIAN_POINT ( 'NONE',  ( 49.97728705011488870, 45.49948385550240459, -6.000000000000000888 ) ) ;
#9855 = CARTESIAN_POINT ( 'NONE',  ( -74.99999999999997158, 40.00000000000001421, 10.00000000000000000 ) ) ;
#9856 = ORIENTED_EDGE ( 'NONE', *, *, #13515, .T. ) ;
#9857 = VERTEX_POINT ( 'NONE', #8003 ) ;
#9858 = VERTEX_POINT ( 'NONE', #3779 ) ;
#9859 = DIRECTION ( 'NONE',  ( -0.000000000000000000, -0.000000000000000000, -1.000000000000000000 ) ) ;
#9860 = VECTOR ( 'NONE', #8592, 1000.000000000000000 ) ;
#9861 = LINE ( 'NONE', #1475, #12013 ) ;
#9862 = FACE_OUTER_BOUND ( 'NONE', #4813, .T. ) ;
#9863 = DIRECTION ( 'NONE',  ( -1.000000000000000000, -0.000000000000000000, -0.000000000000000000 ) ) ;
#9864 = FACE_OUTER_BOUND ( 'NONE', #7471, .T. ) ;
#9865 = CARTESIAN_POINT ( 'NONE',  ( 56.66441430157294690, 52.90051614449765793, -2.141517661632166281 ) ) ;
#9866 = CARTESIAN_POINT ( 'NONE',  ( 2.899426713160750069, -23.82535289025860337, -8.999999999999996447 ) ) ;
#9867 = CARTESIAN_POINT ( 'NONE',  ( 43.33558569842703179, 53.09948385550240602, -2.141517661632099223 ) ) ;
#9868 = CARTESIAN_POINT ( 'NONE',  ( 4.000000000000000000, 2.309401076758497151, -3.433295621305379353 ) ) ;
#9869 = CARTESIAN_POINT ( 'NONE',  ( 42.38452918213188525, 63.09948385550240602, -2.450534656007040013 ) ) ;
#9870 = ORIENTED_EDGE ( 'NONE', *, *, #5617, .F. ) ;
#9871 = ORIENTED_EDGE ( 'NONE', *, *, #9017, .T. ) ;
#9872 = CARTESIAN_POINT ( 'NONE',  ( 75.00000000000001421, 2.602085213965211904E-14, 0.000000000000000000 ) ) ;
#9873 = ORIENTED_EDGE ( 'NONE', *, *, #11405, .T. ) ;
#9874 = CARTESIAN_POINT ( 'NONE',  ( 0.000000000000000000, 3.755786496842903495E-16, 3.500000000000000000 ) ) ;
#9875 = CARTESIAN_POINT ( 'NONE',  ( 9.999999999999994671, 20.00000000000001421, -15.00000000000000000 ) ) ;
#9876 = CARTESIAN_POINT ( 'NONE',  ( 51.92680522751238925, 53.40051614449765793, 6.007379884777208190 ) ) ;
#9877 = CARTESIAN_POINT ( 'NONE',  ( -0.6666666666666651864, 4.233901974057260098, -3.300726591567081147 ) ) ;
#9878 = CARTESIAN_POINT ( 'NONE',  ( 57.61547081786812896, 56.09948385550240602, 2.450534656007040901 ) ) ;
#9879 = CARTESIAN_POINT ( 'NONE',  ( 47.70284917648453415, 55.39948385550238896, -6.992620115222774047 ) ) ;
#9880 = DIRECTION ( 'NONE',  ( -0.000000000000000000, -0.000000000000000000, 1.000000000000000000 ) ) ;
#9881 = ADVANCED_FACE ( 'NONE', ( #8141 ), #4876, .F. ) ;
#9882 = CARTESIAN_POINT ( 'NONE',  ( 52.62207051974829852, 60.60051614449765367, -7.992620115222797139 ) ) ;
#9883 = ORIENTED_EDGE ( 'NONE', *, *, #7281, .F. ) ;
#9884 = ORIENTED_EDGE ( 'NONE', *, *, #12852, .T. ) ;
#9885 = ORIENTED_EDGE ( 'NONE', *, *, #12034, .F. ) ;
#9886 = VECTOR ( 'NONE', #10168, 1000.000000000000000 ) ;
#9887 = VERTEX_POINT ( 'NONE', #5800 ) ;
#9888 = CYLINDRICAL_SURFACE ( 'NONE', #5163, 2.649999999999988365 ) ;
#9889 = CARTESIAN_POINT ( 'NONE',  ( 4.000000000000000000, 0.000000000000000000, 0.000000000000000000 ) ) ;
#9890 = EDGE_CURVE ( 'NONE', #1754, #8976, #9997, .T. ) ;
#9891 = CARTESIAN_POINT ( 'NONE',  ( 13.99999999999999822, 0.000000000000000000, 0.000000000000000000 ) ) ;
#9892 = EDGE_CURVE ( 'NONE', #9621, #8787, #3709, .T. ) ;
#9893 = CARTESIAN_POINT ( 'NONE',  ( 55.71335778527780747, 56.09948385550240602, 1.832500667257165983 ) ) ;
#9894 = CARTESIAN_POINT ( 'NONE',  ( 54.09612160359792199, 45.30051614449766362, 5.676469297603124353 ) ) ;
#9895 = EDGE_CURVE ( 'NONE', #6264, #11796, #13234, .T. ) ;
#9896 = CARTESIAN_POINT ( 'NONE',  ( 57.60143344285435774, 53.10051614449767499, 2.493737253992045044 ) ) ;
#9897 = EDGE_CURVE ( 'NONE', #4643, #8775, #12557, .T. ) ;
#9898 = CIRCLE ( 'NONE', #830, 2.649999999999985700 ) ;
#9899 = DIRECTION ( 'NONE',  ( 1.000000000000000000, 0.000000000000000000, 0.000000000000000000 ) ) ;
#9900 = CYLINDRICAL_SURFACE ( 'NONE', #4932, 12.50000000000000000 ) ;
#9901 = CARTESIAN_POINT ( 'NONE',  ( 56.65037692655921120, 63.10051614449766078, 2.184720259617097593 ) ) ;
#9902 = AXIS2_PLACEMENT_3D ( 'NONE', #5578, #2445, #6684 ) ;
#9903 = ORIENTED_EDGE ( 'NONE', *, *, #3560, .F. ) ;
#9904 = DIRECTION ( 'NONE',  ( 0.000000000000000000, 0.000000000000000000, 1.000000000000000000 ) ) ;
#9905 = EDGE_LOOP ( 'NONE', ( #1714, #2946, #10120, #7553 ) ) ;
#9906 = CONICAL_SURFACE ( 'NONE', #9697, 3.500000000000000000, 1.047197551196600296 ) ;
#9907 = CARTESIAN_POINT ( 'NONE',  ( 22.14999999999999858, -20.00000000000000000, -20.00000000000000000 ) ) ;
#9908 = DIRECTION ( 'NONE',  ( -0.000000000000000000, 0.000000000000000000, 1.000000000000000000 ) ) ;
#9909 = DIRECTION ( 'NONE',  ( 0.000000000000000000, 0.000000000000000000, 1.000000000000000000 ) ) ;
#9910 = CARTESIAN_POINT ( 'NONE',  ( 52.29715082351547295, 56.39948385550238896, 6.992620115222774047 ) ) ;
#9911 = EDGE_CURVE ( 'NONE', #3730, #2660, #788, .T. ) ;
#9912 = CARTESIAN_POINT ( 'NONE',  ( 53.50833635130544508, 59.30051614449766362, 4.867452303228181343 ) ) ;
#9913 = CARTESIAN_POINT ( 'NONE',  ( 4.175813232069150338, -4.122719923832746325, 2.362127131240695889E-16 ) ) ;
#9914 = LINE ( 'NONE', #9786, #7711 ) ;
#9915 = CARTESIAN_POINT ( 'NONE',  ( 44.91013252490150620, 62.20051614449766220, -3.727524721679154940 ) ) ;
#9916 = CARTESIAN_POINT ( 'NONE',  ( 52.25172492374522903, 63.59948385550237759, -7.007379884777225953 ) ) ;
#9917 = CARTESIAN_POINT ( 'NONE',  ( -29.99999999999999645, -40.00000000000000000, 10.00000000000000000 ) ) ;
#9918 = EDGE_LOOP ( 'NONE', ( #5688, #12098, #10301, #13480 ) ) ;
#9919 = UNCERTAINTY_MEASURE_WITH_UNIT (LENGTH_MEASURE( 1.000000000000000082E-05 ), #10825, 'distance_accuracy_value', 'NONE');
#9920 = VERTEX_POINT ( 'NONE', #3089 ) ;
#9921 = DIRECTION ( 'NONE',  ( -1.000000000000000000, 0.000000000000000000, -0.000000000000000000 ) ) ;
#9922 = DIRECTION ( 'NONE',  ( -1.000000000000000000, 0.000000000000000000, 0.000000000000000000 ) ) ;
#9923 = EDGE_CURVE ( 'NONE', #13190, #5173, #12793, .T. ) ;
#9924 = LINE ( 'NONE', #6627, #3341 ) ;
#9925 = AXIS2_PLACEMENT_3D ( 'NONE', #450, #2328, #10765 ) ;
#9926 = LINE ( 'NONE', #6822, #4254 ) ;
#9927 = DIRECTION ( 'NONE',  ( 0.000000000000000000, 0.000000000000000000, 1.000000000000000000 ) ) ;
#9928 = ADVANCED_FACE ( 'NONE', ( #11595 ), #13646, .T. ) ;
#9929 = CARTESIAN_POINT ( 'NONE',  ( 49.97728705011495265, 51.50051614449765935, 7.000000000000000888 ) ) ;
#9930 = ADVANCED_FACE ( 'NONE', ( #10482 ), #7384, .T. ) ;
#9931 = DIRECTION ( 'NONE',  ( 0.000000000000000000, 0.000000000000000000, -1.000000000000000000 ) ) ;
#9932 = CARTESIAN_POINT ( 'NONE',  ( 55.96859303347804371, 52.19948385550240033, 4.306917132069425946 ) ) ;
#9933 = CARTESIAN_POINT ( 'NONE',  ( 52.25172492374522903, 45.59948385550240602, -7.007379884777225953 ) ) ;
#9934 = CARTESIAN_POINT ( 'NONE',  ( 56.65037692655918988, 45.89948385550240317, -2.184720259617163762 ) ) ;
#9935 = VECTOR ( 'NONE', #5486, 1000.000000000000000 ) ;
#9936 = CIRCLE ( 'NONE', #8184, 1.499999999999998446 ) ;
#9937 = ORIENTED_EDGE ( 'NONE', *, *, #5940, .T. ) ;
#9938 = ORIENTED_EDGE ( 'NONE', *, *, #13384, .T. ) ;
#9939 = CARTESIAN_POINT ( 'NONE',  ( 4.086375874528100027, -2.103253014742892280, -3.499999999999999556 ) ) ;
#9940 = ORIENTED_EDGE ( 'NONE', *, *, #12212, .T. ) ;
#9941 = CARTESIAN_POINT ( 'NONE',  ( 6.244297270355322560, -0.4917101305082151597, -5.105276777067913052 ) ) ;
#9942 = DIRECTION ( 'NONE',  ( 0.000000000000000000, 0.000000000000000000, 1.000000000000000000 ) ) ;
#9943 = CARTESIAN_POINT ( 'NONE',  ( 46.49166364869456913, 56.30051614449766362, -4.867452303228181343 ) ) ;
#9944 = VECTOR ( 'NONE', #5339, 1000.000000000000000 ) ;
#9945 = CARTESIAN_POINT ( 'NONE',  ( -65.14999999999996305, 32.50000000000001421, 15.00000000000000000 ) ) ;
#9946 = CARTESIAN_POINT ( 'NONE',  ( 52.57664461997811856, 55.59948385550240602, -8.007379884777229506 ) ) ;
#9947 = CARTESIAN_POINT ( 'NONE',  ( 56.65037692655918988, 57.89948385550240317, -2.184720259617163762 ) ) ;
#9948 = DIRECTION ( 'NONE',  ( 1.000000000000000000, 0.000000000000000000, 0.000000000000000000 ) ) ;
#9949 = CARTESIAN_POINT ( 'NONE',  ( 54.68390685589039890, 63.30051614449767072, 6.485486291978072693 ) ) ;
#9951 = EDGE_CURVE ( 'NONE', #278, #13382, #9447, .T. ) ;
#9950 = VERTEX_POINT ( 'NONE', #1907 ) ;
#9952 = CONTEXT_DEPENDENT_SHAPE_REPRESENTATION ( #6218, #4453 ) ;
#9953 = AXIS2_PLACEMENT_3D ( 'NONE', #10341, #7026, #9243 ) ;
#9954 = ORIENTED_EDGE ( 'NONE', *, *, #4684, .T. ) ;
#9955 = ORIENTED_EDGE ( 'NONE', *, *, #832, .F. ) ;
#9956 = VERTEX_POINT ( 'NONE', #3158 ) ;
#9957 = CARTESIAN_POINT ( 'NONE',  ( 6.534838248920899595, 5.903531555104835071, 8.098083288904839678E-18 ) ) ;
#9958 = DIRECTION ( 'NONE',  ( -0.000000000000000000, -0.000000000000000000, -1.000000000000000000 ) ) ;
#9959 = EDGE_CURVE ( 'NONE', #5207, #1369, #11028, .T. ) ;
#9960 = CARTESIAN_POINT ( 'NONE',  ( 2.000000000000000000, 0.000000000000000000, 0.000000000000000000 ) ) ;
#9961 = CARTESIAN_POINT ( 'NONE',  ( 48.02776887271745210, 53.39948385550241028, -5.992620115222778487 ) ) ;
#9962 = DIRECTION ( 'NONE',  ( 0.000000000000000000, 0.000000000000000000, -1.000000000000000000 ) ) ;
#9963 = CARTESIAN_POINT ( 'NONE',  ( 56.79116909180259398, 51.20051614449766220, 4.963592699178938972 ) ) ;
#9964 = AXIS2_PLACEMENT_3D ( 'NONE', #9960, #8664, #2285 ) ;
#9965 = DIRECTION ( 'NONE',  ( 1.000000000000000000, 0.000000000000000000, 0.000000000000000000 ) ) ;
#9966 = AXIS2_PLACEMENT_3D ( 'NONE', #2294, #8740, #11905 ) ;
#9967 = CYLINDRICAL_SURFACE ( 'NONE', #10212, 4.000000000000000000 ) ;
#9968 = CARTESIAN_POINT ( 'NONE',  ( 47.70284917648459100, 61.60051614449764656, 6.992620115222796251 ) ) ;
#9969 = ORIENTED_EDGE ( 'NONE', *, *, #2529, .F. ) ;
#9970 = CYLINDRICAL_SURFACE ( 'NONE', #7301, 6.080745460913608902 ) ;
#9971 = VERTEX_POINT ( 'NONE', #2044 ) ;
#9972 = CIRCLE ( 'NONE', #10206, 0.5999999999999980904 ) ;
#9973 = VECTOR ( 'NONE', #12668, 1000.000000000000000 ) ;
#9974 = DIRECTION ( 'NONE',  ( 0.000000000000000000, 0.000000000000000000, -1.000000000000000000 ) ) ;
#9975 = DIRECTION ( 'NONE',  ( -0.000000000000000000, -0.000000000000000000, -1.000000000000000000 ) ) ;
#9976 = CARTESIAN_POINT ( 'NONE',  ( 52.25172492374522903, 55.59948385550241312, -7.007379884777225953 ) ) ;
#9977 = CARTESIAN_POINT ( 'NONE',  ( 51.97223112728249816, 56.60051614449765367, -5.992620115222793586 ) ) ;
#9978 = DIRECTION ( 'NONE',  ( 0.000000000000000000, 0.000000000000000000, 1.000000000000000000 ) ) ;
#9979 = CARTESIAN_POINT ( 'NONE',  ( 0.1999999999999987899, 0.000000000000000000, 0.000000000000000000 ) ) ;
#9980 = CARTESIAN_POINT ( 'NONE',  ( 46.45491332379576477, 61.70051614449766220, 4.840751629271188961 ) ) ;
#9981 = CARTESIAN_POINT ( 'NONE',  ( 46.45491332379572924, 49.29948385550240886, -4.840751629271157874 ) ) ;
#9982 = LINE ( 'NONE', #7018, #2520 ) ;
#9983 = ORIENTED_EDGE ( 'NONE', *, *, #9584, .F. ) ;
#9984 = VECTOR ( 'NONE', #7284, 1000.000000000000000 ) ;
#9986 = EDGE_CURVE ( 'NONE', #2102, #3637, #5095, .T. ) ;
#9985 = EDGE_LOOP ( 'NONE', ( #376, #8759 ) ) ;
#9987 = DIRECTION ( 'NONE',  ( 1.000000000000000000, 0.000000000000000000, 0.000000000000000000 ) ) ;
#9988 = B_SPLINE_CURVE_WITH_KNOTS ( 'NONE', 3,
 ( #12224, #5811, #8849, #5672, #2825, #10008 ),
 .UNSPECIFIED., .F., .F.,
 ( 4, 2, 4 ),
 ( 0.002044882221487534079, 0.003063384235218496315, 0.004081886248949458985 ),
 .UNSPECIFIED. ) ;
#9989 = EDGE_CURVE ( 'NONE', #5130, #3296, #12416, .T. ) ;
#9990 = CARTESIAN_POINT ( 'NONE',  ( 3.436319922986518449, -2.634841920959471562, -3.531542292954761741 ) ) ;
#9991 = FACE_OUTER_BOUND ( 'NONE', #3265, .T. ) ;
#9992 = CARTESIAN_POINT ( 'NONE',  ( 6.390983399715593372, 5.837459000499768180, -0.1107755759658281131 ) ) ;
#9993 = ADVANCED_FACE ( 'NONE', ( #13583 ), #1493, .F. ) ;
#9994 = DIRECTION ( 'NONE',  ( -1.000000000000000000, 0.000000000000000000, 0.000000000000000000 ) ) ;
#9995 = VECTOR ( 'NONE', #12095, 1000.000000000000000 ) ;
#9996 = CARTESIAN_POINT ( 'NONE',  ( 44.03140696652198471, 59.80051614449766362, 4.306917132069485454 ) ) ;
#9997 = LINE ( 'NONE', #515, #8407 ) ;
#9998 = DIRECTION ( 'NONE',  ( 1.000000000000000000, 0.000000000000000000, 0.000000000000000000 ) ) ;
#9999 = CARTESIAN_POINT ( 'NONE',  ( 44.03140696652192787, 51.19948385550238612, -4.306917132069425058 ) ) ;
#10000 = CARTESIAN_POINT ( 'NONE',  ( 45.86712807150323812, 47.29948385550240886, -5.649768623646098220 ) ) ;
#10001 = CARTESIAN_POINT ( 'NONE',  ( 49.97728705011486738, 63.49948385550241170, -8.000000000000001776 ) ) ;
#10002 = ORIENTED_EDGE ( 'NONE', *, *, #3284, .F. ) ;
#10003 = VERTEX_POINT ( 'NONE', #3986 ) ;
#10004 = CARTESIAN_POINT ( 'NONE',  ( 4.180345136606690382, -2.085999704580137060, -3.570468642550115312 ) ) ;
#10005 = B_SPLINE_CURVE_WITH_KNOTS ( 'NONE', 3,
 ( #7072, #2920, #11352, #1874, #10312 ),
 .UNSPECIFIED., .F., .F.,
 ( 4, 1, 4 ),
 ( 0.000000000000000000, 0.002020725942163690506, 0.004041451884327381013 ),
 .UNSPECIFIED. ) ;
#10006 = VERTEX_POINT ( 'NONE', #11653 ) ;
#10007 = B_SPLINE_CURVE_WITH_KNOTS ( 'NONE', 3,
 ( #5440, #3550, #8744, #6477, #10679, #5499 ),
 .UNSPECIFIED., .F., .F.,
 ( 4, 2, 4 ),
 ( -3.640115492407174633E-06, 0.0002066546034006553863, 0.0004169493222937179812 ),
 .UNSPECIFIED. ) ;
#10008 = CARTESIAN_POINT ( 'NONE',  ( 0.3126073911696399255, 2.020725942163686284, -3.499999999999999556 ) ) ;
#10009 = LINE ( 'NONE', #13315, #6194 ) ;
#10010 = CARTESIAN_POINT ( 'NONE',  ( 44.88205777487401349, 59.80051614449766362, 3.688883143319584779 ) ) ;
#10011 = CARTESIAN_POINT ( 'NONE',  ( -4.198928548860774157, 0.8158838809860065044, -3.526471437616918170 ) ) ;
#10012 = CARTESIAN_POINT ( 'NONE',  ( 47.42335538002188144, 54.59948385550240602, 8.007379884777233059 ) ) ;
#10013 = EDGE_CURVE ( 'NONE', #12709, #4695, #5644, .T. ) ;
#10014 = CARTESIAN_POINT ( 'NONE',  ( 54.09612160359786515, 59.69948385550240033, -5.676469297603166098 ) ) ;
#10015 = CARTESIAN_POINT ( 'NONE',  ( 6.196878017913830305, 1.924500897298746960, -4.999999999999999112 ) ) ;
#10016 = CIRCLE ( 'NONE', #759, 8.099999999999999645 ) ;
#10017 = CARTESIAN_POINT ( 'NONE',  ( 45.27934281921082516, 61.70051614449766220, 6.458785618021089192 ) ) ;
#10018 = VERTEX_POINT ( 'NONE', #7246 ) ;
#10019 = ORIENTED_EDGE ( 'NONE', *, *, #12581, .T. ) ;
#10020 = VERTEX_POINT ( 'NONE', #8284 ) ;
#10021 = VERTEX_POINT ( 'NONE', #11452 ) ;
#10022 = ADVANCED_FACE ( 'NONE', ( #9585 ), #1326, .T. ) ;
#10023 = CARTESIAN_POINT ( 'NONE',  ( 30.00000000000000355, 40.00000000000000000, 10.00000000000000000 ) ) ;
#10025 = CIRCLE ( 'NONE', #7177, 15.00000000000000000 ) ;
#10024 = SHAPE_REPRESENTATION_RELATIONSHIP ( 'NONE' , 'NONE' ,  #10956, #5696 ) ;
#10026 = DIRECTION ( 'NONE',  ( 1.000000000000000000, 0.000000000000000000, 0.000000000000000000 ) ) ;
#10027 = CARTESIAN_POINT ( 'NONE',  ( 20.00000000000000000, -20.00000000000000000, -23.00000000000000000 ) ) ;
#10028 = LINE ( 'NONE', #8175, #10959 ) ;
#10029 = CARTESIAN_POINT ( 'NONE',  ( 46.45491332379572924, 59.29948385550240886, -4.840751629271157874 ) ) ;
#10030 = CARTESIAN_POINT ( 'NONE',  ( 56.65037692655921120, 49.10051614449766078, 2.184720259617097593 ) ) ;
#10031 = CIRCLE ( 'NONE', #8287, 2.500000000000000444 ) ;
#10032 = CARTESIAN_POINT ( 'NONE',  ( 45.31609314410960820, 52.30051614449766362, -6.485486291978072693 ) ) ;
#10033 = DIRECTION ( 'NONE',  ( 0.000000000000000000, 0.000000000000000000, -1.000000000000000000 ) ) ;
#10034 = DIRECTION ( 'NONE',  ( -0.000000000000000000, -0.000000000000000000, 1.000000000000000000 ) ) ;
#10035 = CARTESIAN_POINT ( 'NONE',  ( 57.36023556966787851, 63.00051614449767357, 0.02388180880515038476 ) ) ;
#10036 = PRODUCT_DEFINITION ( 'UNKNOWN', '', #6841, #11358 ) ;
#10037 = ORIENTED_EDGE ( 'NONE', *, *, #1753, .T. ) ;
#10038 = DIRECTION ( 'NONE',  ( -0.000000000000000000, 0.000000000000000000, -1.000000000000000000 ) ) ;
#10039 = ORIENTED_EDGE ( 'NONE', *, *, #12932, .T. ) ;
#10040 = DIRECTION ( 'NONE',  ( -1.000000000000000000, -0.000000000000000000, -0.000000000000000000 ) ) ;
#10041 = DIRECTION ( 'NONE',  ( -0.000000000000000000, 0.000000000000000000, -1.000000000000000000 ) ) ;
#10042 =( NAMED_UNIT ( * ) PLANE_ANGLE_UNIT ( ) SI_UNIT ( $, .RADIAN. ) );
#10043 = CARTESIAN_POINT ( 'NONE',  ( 44.03140696652192787, 55.19948385550238612, -4.306917132069425058 ) ) ;
#10044 = CARTESIAN_POINT ( 'NONE',  ( 42.63976443033212149, 54.99948385550239749, 0.02388180880522514787 ) ) ;
#10045 = DIRECTION ( 'NONE',  ( -0.7071067811865350272, 0.000000000000000000, 0.7071067811865598962 ) ) ;
#10046 = DIRECTION ( 'NONE',  ( -0.000000000000000000, 0.8660254037844392627, 0.4999999999999990008 ) ) ;
#10047 = FACE_OUTER_BOUND ( 'NONE', #11631, .T. ) ;
#10048 = CARTESIAN_POINT ( 'NONE',  ( 45.86712807150329496, 45.70051614449766220, 5.649768623646139964 ) ) ;
#10049 = CARTESIAN_POINT ( 'NONE',  ( 43.69122665457040000, 48.99948385550241170, 0.02388180880521036456 ) ) ;
#10050 = CARTESIAN_POINT ( 'NONE',  ( -4.999999999999998224, -20.00000000000000000, 15.00000000000000355 ) ) ;
#10051 = ORIENTED_EDGE ( 'NONE', *, *, #8387, .T. ) ;
#10052 = ORIENTED_EDGE ( 'NONE', *, *, #40, .F. ) ;
#10053 = ORIENTED_EDGE ( 'NONE', *, *, #6993, .T. ) ;
#10054 = CARTESIAN_POINT ( 'NONE',  ( 12.17636723815389566, -28.75991329190035373, -9.000000000000000000 ) ) ;
#10055 = CARTESIAN_POINT ( 'NONE',  ( 2.687328764639642653, -3.067272167851299969, -0.05923475698271395140 ) ) ;
#10056 = LINE ( 'NONE', #571, #11953 ) ;
#10057 =( NAMED_UNIT ( * ) PLANE_ANGLE_UNIT ( ) SI_UNIT ( $, .RADIAN. ) );
#10058 = CARTESIAN_POINT ( 'NONE',  ( 6.390820841722129941, 2.823237767533145703, 5.110008744785254464 ) ) ;
#10059 = DIRECTION ( 'NONE',  ( 1.000000000000000000, 0.000000000000000000, 0.000000000000000000 ) ) ;
#10060 = ADVANCED_FACE ( 'NONE', ( #6485 ), #6549, .T. ) ;
#10061 = CARTESIAN_POINT ( 'NONE',  ( 52.25172492374527877, 59.40051614449765083, 7.007379884777203749 ) ) ;
#10062 = CARTESIAN_POINT ( 'NONE',  ( 0.04201760816084261496, -0.9730571234389092661, -5.000000000000000888 ) ) ;
#10063 = ADVANCED_FACE ( 'NONE', ( #12946 ), #171, .T. ) ;
#10064 = CARTESIAN_POINT ( 'NONE',  ( 3.951447005078450037, 2.357513599190969256, -2.916666666666667407 ) ) ;
#10065 = CARTESIAN_POINT ( 'NONE',  ( 54.13287192849676188, 60.29948385550240886, 5.649768623646098220 ) ) ;
#10066 = ADVANCED_FACE ( 'NONE', ( #7580 ), #9783, .T. ) ;
#10067 = CARTESIAN_POINT ( 'NONE',  ( 43.33558569842703179, 49.09948385550240602, -2.141517661632099223 ) ) ;
#10068 = CIRCLE ( 'NONE', #9192, 1.500000000000001332 ) ;
#10069 = EDGE_CURVE ( 'NONE', #11878, #10020, #9936, .T. ) ;
#10070 = CARTESIAN_POINT ( 'NONE',  ( 57.36023556966787851, 51.99948385550238328, -0.02388180880522424582 ) ) ;
#10071 = VECTOR ( 'NONE', #4719, 1000.000000000000000 ) ;
#10072 = EDGE_LOOP ( 'NONE', ( #11095, #6393 ) ) ;
#10073 = ORIENTED_EDGE ( 'NONE', *, *, #3170, .F. ) ;
#10074 = LINE ( 'NONE', #4696, #5939 ) ;
#10075 = ADVANCED_FACE ( 'NONE', ( #9717 ), #4530, .F. ) ;
#10076 = VERTEX_POINT ( 'NONE', #10749 ) ;
#10077 = DIRECTION ( 'NONE',  ( -0.000000000000000000, -0.000000000000000000, 1.000000000000000000 ) ) ;
#10078 = CARTESIAN_POINT ( 'NONE',  ( 4.050823680195224874, 3.779313952391379239, -0.5899027668435166127 ) ) ;
#10079 = CARTESIAN_POINT ( 'NONE',  ( 53.54508667620424234, 60.70051614449766930, -4.840751629271188961 ) ) ;
#10080 = CARTESIAN_POINT ( 'NONE',  ( 6.196878017913830305, 3.367876570272813730, 4.166666666666666075 ) ) ;
#10081 = ADVANCED_FACE ( 'NONE', ( #1201 ), #10810, .F. ) ;
#10082 = CARTESIAN_POINT ( 'NONE',  ( 52.62207051974839089, 62.39948385550240317, 7.992620115222770494 ) ) ;
#10083 = EDGE_CURVE ( 'NONE', #6658, #2470, #3996, .T. ) ;
#10084 = CARTESIAN_POINT ( 'NONE',  ( 55.96859303347804371, 62.19948385550240744, 4.306917132069425946 ) ) ;
#10085 = PLANE ( 'NONE',  #4272 ) ;
#10086 = CARTESIAN_POINT ( 'NONE',  ( 58.41169779390614281, 45.99948385550240459, -0.02388180880523160798 ) ) ;
#10087 = ORIENTED_EDGE ( 'NONE', *, *, #10150, .F. ) ;
#10088 = EDGE_LOOP ( 'NONE', ( #4829, #13296, #8293 ) ) ;
#10089 = EDGE_LOOP ( 'NONE', ( #13555, #7242, #7590, #3938, #6538, #11538, #8169, #3808, #6172, #164 ) ) ;
#10090 = ORIENTED_EDGE ( 'NONE', *, *, #9063, .F. ) ;
#10091 = FACE_OUTER_BOUND ( 'NONE', #3466, .T. ) ;
#10092 = FACE_OUTER_BOUND ( 'NONE', #1716, .T. ) ;
#10093 = DIRECTION ( 'NONE',  ( -1.000000000000000000, -0.000000000000000000, -0.000000000000000000 ) ) ;
#10094 = DIRECTION ( 'NONE',  ( 1.000000000000000000, 0.000000000000000000, 0.000000000000000000 ) ) ;
#10095 = DIRECTION ( 'NONE',  ( -1.000000000000000000, 0.000000000000000000, 0.000000000000000000 ) ) ;
#10096 = CARTESIAN_POINT ( 'NONE',  ( 51.92680522751233951, 61.59948385550240602, -6.007379884777223289 ) ) ;
#10097 = CARTESIAN_POINT ( 'NONE',  ( 43.33558569842706021, 53.90051614449765793, 2.141517661632167169 ) ) ;
#10098 = CARTESIAN_POINT ( 'NONE',  ( 58.41169779390614281, 55.00051614449766646, 0.02388180880515032231 ) ) ;
#10099 = ADVANCED_FACE ( 'NONE', ( #11919 ), #2203, .F. ) ;
#10100 = DIRECTION ( 'NONE',  ( -9.710251638871371392E-17, -5.969973981896233748E-17, -1.000000000000000000 ) ) ;
#10101 = CARTESIAN_POINT ( 'NONE',  ( 53.61415392313774220, 44.99999999999997868, -5.449226822604907206 ) ) ;
#10102 = CARTESIAN_POINT ( 'NONE',  ( 56.81924384183006538, 46.80051614449766362, -4.924951120819380357 ) ) ;
#10103 = VECTOR ( 'NONE', #6834, 1000.000000000000000 ) ;
#10105 = ORIENTED_EDGE ( 'NONE', *, *, #8218, .T. ) ;
#10104 = VERTEX_POINT ( 'NONE', #10686 ) ;
#10106 = DIRECTION ( 'NONE',  ( -1.000000000000000000, 0.000000000000000000, 0.000000000000000000 ) ) ;
#10107 = VERTEX_POINT ( 'NONE', #1127 ) ;
#10108 = CARTESIAN_POINT ( 'NONE',  ( 1.734723475976807094E-15, 4.618802153517012954, -0.4999999999999995559 ) ) ;
#10109 = DIRECTION ( 'NONE',  ( 1.000000000000000000, 0.000000000000000000, 0.000000000000000000 ) ) ;
#10110 = DIRECTION ( 'NONE',  ( -0.9768494444719831860, -0.2139279384156685671, 1.428280402131856228E-22 ) ) ;
#10111 = CARTESIAN_POINT ( 'NONE',  ( 42.63976443033212860, 64.99948385550240459, 0.02388180880522514787 ) ) ;
#10112 = VECTOR ( 'NONE', #2453, 1000.000000000000000 ) ;
#10113 = CARTESIAN_POINT ( 'NONE',  ( 54.13287192849676188, 60.29948385550240886, 5.649768623646098220 ) ) ;
#10114 = LINE ( 'NONE', #624, #1136 ) ;
#10115 = PLANE ( 'NONE',  #136 ) ;
#10116 = DIRECTION ( 'NONE',  ( 0.000000000000000000, -1.000000000000000000, 1.345283343056720273E-15 ) ) ;
#10117 = CARTESIAN_POINT ( 'NONE',  ( 56.30877334542961421, 63.00051614449766646, 0.02388180880515774693 ) ) ;
#10118 = CARTESIAN_POINT ( 'NONE',  ( 53.54508667620428497, 52.29948385550240886, 4.840751629271157874 ) ) ;
#10119 = LINE ( 'NONE', #631, #8940 ) ;
#10120 = ORIENTED_EDGE ( 'NONE', *, *, #7819, .T. ) ;
#10121 = AXIS2_PLACEMENT_3D ( 'NONE', #8170, #2983, #4151 ) ;
#10122 = ADVANCED_FACE ( 'NONE', ( #2441 ), #5759, .T. ) ;
#10123 = VERTEX_POINT ( 'NONE', #4327 ) ;
#10124 = VERTEX_POINT ( 'NONE', #5353 ) ;
#10125 = LINE ( 'NONE', #4888, #1278 ) ;
#10126 = MECHANICAL_DESIGN_GEOMETRIC_PRESENTATION_REPRESENTATION (  '', ( #11294 ), #1056 ) ;
#10127 = CARTESIAN_POINT ( 'NONE',  ( 2.712762565639649015, -3.052587955997662306, -3.430618716626630871 ) ) ;
#10128 = CARTESIAN_POINT ( 'NONE',  ( 6.534224484704323821, -2.950930484791555841, 5.111161529262928660 ) ) ;
#10129 = DIRECTION ( 'NONE',  ( 0.000000000000000000, 0.000000000000000000, 1.000000000000000000 ) ) ;
#10130 = DIRECTION ( 'NONE',  ( -1.000000000000000000, -0.000000000000000000, -0.000000000000000000 ) ) ;
#10131 = EDGE_CURVE ( 'NONE', #8730, #11305, #3201, .T. ) ;
#10132 =( GEOMETRIC_REPRESENTATION_CONTEXT ( 3 ) GLOBAL_UNCERTAINTY_ASSIGNED_CONTEXT ( ( #12954 ) ) GLOBAL_UNIT_ASSIGNED_CONTEXT ( ( #6354, #10747, #10684 ) ) REPRESENTATION_CONTEXT ( 'NONE', 'WORKASPACE' ) );
#10133 = CARTESIAN_POINT ( 'NONE',  ( 55.94051828345053679, 59.20051614449766220, 4.345558710429044069 ) ) ;
#10134 = CIRCLE ( 'NONE', #6617, 5.200000000000001066 ) ;
#10135 = CARTESIAN_POINT ( 'NONE',  ( 0.4465819873849485311, -2.886751345948517677, -5.000000000000000000 ) ) ;
#10136 = CARTESIAN_POINT ( 'NONE',  ( 51.97223112728249816, 48.60051614449766788, -5.992620115222793586 ) ) ;
#10137 = FACE_OUTER_BOUND ( 'NONE', #5601, .T. ) ;
#10138 = CARTESIAN_POINT ( 'NONE',  ( 45.86712807150323812, 59.29948385550240175, -5.649768623646098220 ) ) ;
#10139 = CARTESIAN_POINT ( 'NONE',  ( 43.33558569842703179, 53.09948385550240602, -2.141517661632099223 ) ) ;
#10140 = CARTESIAN_POINT ( 'NONE',  ( 52.25172492374522903, 49.59948385550240602, -7.007379884777225953 ) ) ;
#10141 = ADVANCED_FACE ( 'NONE', ( #4306 ), #11425, .T. ) ;
#10142 = VERTEX_POINT ( 'NONE', #7488 ) ;
#10143 = VERTEX_POINT ( 'NONE', #12661 ) ;
#10144 = AXIS2_PLACEMENT_3D ( 'NONE', #10616, #38, #4263 ) ;
#10145 = CARTESIAN_POINT ( 'NONE',  ( 4.052416734886645777, -1.393505408945131308, -3.567979131523694836 ) ) ;
#10146 = AXIS2_PLACEMENT_3D ( 'NONE', #7368, #8594, #3272 ) ;
#10147 = ORIENTED_EDGE ( 'NONE', *, *, #687, .T. ) ;
#10148 = ADVANCED_FACE ( 'NONE', ( #6332 ), #4106, .F. ) ;
#10149 = DIRECTION ( 'NONE',  ( 0.000000000000000000, 0.000000000000000000, -1.000000000000000000 ) ) ;
#10150 = EDGE_CURVE ( 'NONE', #12408, #6051, #8113, .T. ) ;
#10151 = DIRECTION ( 'NONE',  ( 1.000000000000000000, 0.000000000000000000, 0.000000000000000000 ) ) ;
#10152 = CARTESIAN_POINT ( 'NONE',  ( 55.11794222512599362, 58.80051614449766362, -3.688883143319583446 ) ) ;
#10153 = DIRECTION ( 'NONE',  ( 0.000000000000000000, 0.000000000000000000, -1.000000000000000000 ) ) ;
#10154 = CARTESIAN_POINT ( 'NONE',  ( 42.38452918213188525, 57.09948385550240602, -2.450534656007040013 ) ) ;
#10155 = AXIS2_PLACEMENT_3D ( 'NONE', #2531, #7600, #324 ) ;
#10156 = CARTESIAN_POINT ( 'NONE',  ( 54.13287192849676188, 60.29948385550240886, 5.649768623646098220 ) ) ;
#10157 = DIRECTION ( 'NONE',  ( 0.4999999999999977796, 0.8660254037844398178, 0.000000000000000000 ) ) ;
#10158 = CARTESIAN_POINT ( 'NONE',  ( 57.61547081786812896, 50.09948385550240602, 2.450534656007040901 ) ) ;
#10159 = MANIFOLD_SOLID_BREP ( 'AdvancedHole2', #3608 ) ;
#10160 = VERTEX_POINT ( 'NONE', #7225 ) ;
#10161 = CONTEXT_DEPENDENT_SHAPE_REPRESENTATION ( #4700, #10637 ) ;
#10162 = VERTEX_POINT ( 'NONE', #13559 ) ;
#10163 = APPLICATION_CONTEXT ( 'automotive_design' ) ;
#10164 = VERTEX_POINT ( 'NONE', #12532 ) ;
#10165 = ORIENTED_EDGE ( 'NONE', *, *, #5605, .F. ) ;
#10166 = CARTESIAN_POINT ( 'NONE',  ( -20.00000000000000000, -19.99999999999999289, -20.00000000000000000 ) ) ;
#10167 =( GEOMETRIC_REPRESENTATION_CONTEXT ( 3 ) GLOBAL_UNCERTAINTY_ASSIGNED_CONTEXT ( ( #8693 ) ) GLOBAL_UNIT_ASSIGNED_CONTEXT ( ( #6178, #2841, #2774 ) ) REPRESENTATION_CONTEXT ( 'NONE', 'WORKASPACE' ) );
#10168 = DIRECTION ( 'NONE',  ( 0.000000000000000000, 1.000000000000000000, -1.345283343056720273E-15 ) ) ;
#10169 = EDGE_CURVE ( 'NONE', #6957, #11811, #3490, .T. ) ;
#10170 = CIRCLE ( 'NONE', #6224, 4.799999999999999822 ) ;
#10171 = CARTESIAN_POINT ( 'NONE',  ( -0.5000000000000000000, -6.429618962271402616, -1.000000000000000000 ) ) ;
#10172 = DIRECTION ( 'NONE',  ( 9.858538378746663627E-23, -5.031452844637890958E-23, 1.000000000000000000 ) ) ;
#10173 = DIRECTION ( 'NONE',  ( -1.000000000000000000, -3.469446951953615175E-16, -0.000000000000000000 ) ) ;
#10174 = CARTESIAN_POINT ( 'NONE',  ( 55.08986747509847248, 59.79948385550240175, -3.727524721679197572 ) ) ;
#10175 = CARTESIAN_POINT ( 'NONE',  ( 54.09612160359792199, 53.30051614449766362, 5.676469297603124353 ) ) ;
#10176 = CARTESIAN_POINT ( 'NONE',  ( 52.57664461997821093, 59.40051614449765793, 8.007379884777206414 ) ) ;
#10177 = CARTESIAN_POINT ( 'NONE',  ( 0.3126073911696408136, 2.020725942163688060, 3.500000000000000000 ) ) ;
#10178 = CARTESIAN_POINT ( 'NONE',  ( 1.000000000000000444, -15.10102051443364246, 9.000000000000000000 ) ) ;
#10179 = CARTESIAN_POINT ( 'NONE',  ( 52.57664461997821093, 49.40051614449766504, 8.007379884777206414 ) ) ;
#10181 = ORIENTED_EDGE ( 'NONE', *, *, #12273, .T. ) ;
#10180 = ORIENTED_EDGE ( 'NONE', *, *, #12525, .F. ) ;
#10182 = CARTESIAN_POINT ( 'NONE',  ( -4.211140560182196957, 2.431303136016537803, -3.745885042887433514 ) ) ;
#10183 = VERTEX_POINT ( 'NONE', #13623 ) ;
#10184 = VERTEX_POINT ( 'NONE', #4170 ) ;
#10185 = DIRECTION ( 'NONE',  ( 0.000000000000000000, 0.000000000000000000, 1.000000000000000000 ) ) ;
#10186 = CARTESIAN_POINT ( 'NONE',  ( 1.925929944387235853E-31, 15.00000000000001599, 9.999999999999998224 ) ) ;
#10187 = AXIS2_PLACEMENT_3D ( 'NONE', #5587, #317, #12008 ) ;
#10188 = ITEM_DEFINED_TRANSFORMATION ( 'NONE', 'NONE', #6204,  #430 ) ;
#10189 = CARTESIAN_POINT ( 'NONE',  ( 56.66441430157296821, 64.09948385550239891, 2.141517661632100111 ) ) ;
#10190 = CARTESIAN_POINT ( 'NONE',  ( 54.09612160359786515, 57.69948385550240744, -5.676469297603166098 ) ) ;
#10191 = CYLINDRICAL_SURFACE ( 'NONE', #7120, 2.649999999999988365 ) ;
#10192 = DIRECTION ( 'NONE',  ( 1.000000000000000000, 0.000000000000000000, 0.000000000000000000 ) ) ;
#10193 = DIRECTION ( 'NONE',  ( 0.1836763462126260182, -0.9829867750086872524, -1.521953536530129242E-22 ) ) ;
#10194 = CARTESIAN_POINT ( 'NONE',  ( 55.94051828345053679, 53.20051614449766220, 4.345558710429044069 ) ) ;
#10195 = CARTESIAN_POINT ( 'NONE',  ( 48.02776887271745210, 53.39948385550241028, -5.992620115222778487 ) ) ;
#10196 = LINE ( 'NONE', #7989, #517 ) ;
#10197 = VERTEX_POINT ( 'NONE', #8392 ) ;
#10198 = AXIS2_PLACEMENT_3D ( 'NONE', #10186, #2999, #11427 ) ;
#10199 = VECTOR ( 'NONE', #1730, 1000.000000000000000 ) ;
#10200 = VERTEX_POINT ( 'NONE', #12599 ) ;
#10201 = ORIENTED_EDGE ( 'NONE', *, *, #11339, .F. ) ;
#10202 = DIRECTION ( 'NONE',  ( -0.7071067811865533459, 0.000000000000000000, 0.7071067811865416886 ) ) ;
#10203 = CARTESIAN_POINT ( 'NONE',  ( 2.449293598294706513E-15, -20.00000000000000000, 9.999999999999998224 ) ) ;
#10204 = CARTESIAN_POINT ( 'NONE',  ( -2.500000000000000888, 0.000000000000000000, -4.974599999999998801 ) ) ;
#10205 = MANIFOLD_SOLID_BREP ( 'Body', #2492 ) ;
#10206 = AXIS2_PLACEMENT_3D ( 'NONE', #4153, #10577, #8377 ) ;
#10207 = LINE ( 'NONE', #7031, #7952 ) ;
#10208 = CARTESIAN_POINT ( 'NONE',  ( 43.69122665457040000, 64.99948385550240459, 0.02388180880521036456 ) ) ;
#10209 = PLANE ( 'NONE',  #974 ) ;
#10210 = CARTESIAN_POINT ( 'NONE',  ( 43.34962307344081012, 56.89948385550240317, 2.184720259617164650 ) ) ;
#10211 = CARTESIAN_POINT ( 'NONE',  ( 52.29715082351547295, 50.39948385550240317, 6.992620115222774047 ) ) ;
#10212 = AXIS2_PLACEMENT_3D ( 'NONE', #1731, #484, #10936 ) ;
#10213 = EDGE_CURVE ( 'NONE', #11355, #486, #2351, .T. ) ;
#10214 = VERTEX_POINT ( 'NONE', #3129 ) ;
#10215 = CARTESIAN_POINT ( 'NONE',  ( 50.02271294988512551, 46.49948385550240459, 7.000000000000000888 ) ) ;
#10216 = ORIENTED_EDGE ( 'NONE', *, *, #9061, .F. ) ;
#10217 = ORIENTED_EDGE ( 'NONE', *, *, #11276, .T. ) ;
#10218 = FACE_OUTER_BOUND ( 'NONE', #12856, .T. ) ;
#10219 = ORIENTED_EDGE ( 'NONE', *, *, #7466, .F. ) ;
#10220 = DIRECTION ( 'NONE',  ( -1.000000000000000000, 0.000000000000000000, 0.000000000000000000 ) ) ;
#10221 = DIRECTION ( 'NONE',  ( -1.000000000000000000, -0.000000000000000000, -0.000000000000000000 ) ) ;
#10222 = FACE_OUTER_BOUND ( 'NONE', #3197, .T. ) ;
#10223 = CARTESIAN_POINT ( 'NONE',  ( 48.07319477248762496, 60.40051614449765793, -6.007379884777208190 ) ) ;
#10224 = CARTESIAN_POINT ( 'NONE',  ( 41.58830220609386430, 56.99948385550241170, 0.02388180880523263147 ) ) ;
#10225 = CARTESIAN_POINT ( 'NONE',  ( 52.29715082351547295, 62.39948385550239607, 6.992620115222774047 ) ) ;
#10226 = FACE_OUTER_BOUND ( 'NONE', #5154, .T. ) ;
#10227 = CARTESIAN_POINT ( 'NONE',  ( 41.58830220609386430, 48.99948385550241170, 0.02388180880523263147 ) ) ;
#10228 = ORIENTED_EDGE ( 'NONE', *, *, #13637, .F. ) ;
#10229 = VERTEX_POINT ( 'NONE', #6660 ) ;
#10230 = ORIENTED_EDGE ( 'NONE', *, *, #3988, .T. ) ;
#10231 = EDGE_CURVE ( 'NONE', #3701, #13024, #4368, .T. ) ;
#10232 = DIRECTION ( 'NONE',  ( 0.000000000000000000, 0.000000000000000000, -1.000000000000000000 ) ) ;
#10233 = DIRECTION ( 'NONE',  ( -0.000000000000000000, 0.000000000000000000, -1.000000000000000000 ) ) ;
#10234 = LINE ( 'NONE', #1722, #2692 ) ;
#10235 = CARTESIAN_POINT ( 'NONE',  ( -7.499999999999923617, -32.99038105676662269, -9.000000000000000000 ) ) ;
#10236 = LINE ( 'NONE', #1583, #4561 ) ;
#10237 = CARTESIAN_POINT ( 'NONE',  ( 55.71335778527780747, 64.09948385550239891, 1.832500667257165983 ) ) ;
#10238 = CARTESIAN_POINT ( 'NONE',  ( 43.34962307344078880, 52.10051614449766078, -2.184720259617096705 ) ) ;
#10239 = AXIS2_PLACEMENT_3D ( 'NONE', #5724, #13161, #9922 ) ;
#10240 = CARTESIAN_POINT ( 'NONE',  ( 57.61547081786810764, 58.90051614449766504, -2.450534656007114176 ) ) ;
#10241 = CARTESIAN_POINT ( 'NONE',  ( -4.000000000000000000, 1.700094919196744270, -3.320312364301766017 ) ) ;
#10242 = ADVANCED_FACE ( 'NONE', ( #2281 ), #11974, .T. ) ;
#10243 = CARTESIAN_POINT ( 'NONE',  ( 41.58830220609386430, 52.00051614449766646, -0.02388180880514929535 ) ) ;
#10244 = ADVANCED_FACE ( 'NONE', ( #2493 ), #1443, .T. ) ;
#10246 = VERTEX_POINT ( 'NONE', #9889 ) ;
#10245 = ORIENTED_EDGE ( 'NONE', *, *, #12989, .T. ) ;
#10247 = ORIENTED_EDGE ( 'NONE', *, *, #9897, .F. ) ;
#10248 = ORIENTED_EDGE ( 'NONE', *, *, #1952, .T. ) ;
#10249 = CIRCLE ( 'NONE', #6082, 15.00000000000000000 ) ;
#10250 = ORIENTED_EDGE ( 'NONE', *, *, #12523, .T. ) ;
#10251 = MANIFOLD_SOLID_BREP ( 'M5 Clearance Hole1', #13084 ) ;
#10252 = DIRECTION ( 'NONE',  ( -0.000000000000000000, -0.000000000000000000, 1.000000000000000000 ) ) ;
#10253 = AXIS2_PLACEMENT_3D ( 'NONE', #3009, #1964, #3145 ) ;
#10254 = CARTESIAN_POINT ( 'NONE',  ( -14.99999999999999645, -20.00000000000005329, -9.000000000000000000 ) ) ;
#10255 = APPLICATION_PROTOCOL_DEFINITION ( 'draft international standard', 'automotive_design', 1998, #11126 ) ;
#10256 = CARTESIAN_POINT ( 'NONE',  ( 46.49166364869460466, 46.69948385550240744, 4.867452303228209765 ) ) ;
#10257 = CARTESIAN_POINT ( 'NONE',  ( 54.09612160359786515, 59.69948385550240033, -5.676469297603166098 ) ) ;
#10258 = AXIS2_PLACEMENT_3D ( 'NONE', #1778, #944, #9401 ) ;
#10259 = DIRECTION ( 'NONE',  ( 0.000000000000000000, 0.000000000000000000, -1.000000000000000000 ) ) ;
#10260 = AXIS2_PLACEMENT_3D ( 'NONE', #5947, #7814, #13178 ) ;
#10261 = FACE_OUTER_BOUND ( 'NONE', #6990, .T. ) ;
#10262 = B_SPLINE_CURVE_WITH_KNOTS ( 'NONE', 3,
 ( #8174, #12502, #10366, #7263, #9404, #10501, #13600, #4144 ),
 .UNSPECIFIED., .F., .F.,
 ( 4, 2, 2, 4 ),
 ( 0.000000000000000000, 0.001493104274552342322, 0.002986208549104684210, 0.005972417098209366684 ),
 .UNSPECIFIED. ) ;
#10263 = CARTESIAN_POINT ( 'NONE',  ( 62.49999999999998579, 45.00000000000001421, 15.00000000000000000 ) ) ;
#10264 = EDGE_CURVE ( 'NONE', #10164, #5892, #3470, .T. ) ;
#10265 = CARTESIAN_POINT ( 'NONE',  ( 56.66441430157294690, 48.90051614449766504, -2.141517661632166281 ) ) ;
#10266 = CARTESIAN_POINT ( 'NONE',  ( 46.49166364869460466, 54.69948385550240033, 4.867452303228209765 ) ) ;
#10267 = LINE ( 'NONE', #10050, #6520 ) ;
#10268 = VERTEX_POINT ( 'NONE', #5690 ) ;
#10269 = ORIENTED_EDGE ( 'NONE', *, *, #2257, .T. ) ;
#10270 = ORIENTED_EDGE ( 'NONE', *, *, #5203, .T. ) ;
#10271 = FACE_OUTER_BOUND ( 'NONE', #1943, .T. ) ;
#10272 = CARTESIAN_POINT ( 'NONE',  ( -6.080745460913608902, 0.5192545390863924082, 0.000000000000000000 ) ) ;
#10273 = ADVANCED_FACE ( 'NONE', ( #12791 ), #283, .T. ) ;
#10274 = CONICAL_SURFACE ( 'NONE', #11787, 4.000000000000000000, 0.8911886515913786111 ) ;
#10275 = DIRECTION ( 'NONE',  ( -1.000000000000000000, 0.000000000000000000, 0.000000000000000000 ) ) ;
#10276 = CARTESIAN_POINT ( 'NONE',  ( 47.70284917648453415, 47.39948385550238896, -6.992620115222774047 ) ) ;
#10277 = CARTESIAN_POINT ( 'NONE',  ( -20.00000000000000000, -19.99999999999999289, -12.00000000000000000 ) ) ;
#10278 = DIRECTION ( 'NONE',  ( 1.000000000000000000, 0.000000000000000000, 0.000000000000000000 ) ) ;
#10279 = CARTESIAN_POINT ( 'NONE',  ( 55.11794222512599362, 44.80051614449766362, -3.688883143319583446 ) ) ;
#10280 = DIRECTION ( 'NONE',  ( 1.000000000000000000, 0.000000000000000000, 0.000000000000000000 ) ) ;
#10281 = CARTESIAN_POINT ( 'NONE',  ( 45.86712807150323812, 55.29948385550240175, -5.649768623646098220 ) ) ;
#10282 = CARTESIAN_POINT ( 'NONE',  ( 43.33558569842703179, 55.09948385550241312, -2.141517661632099223 ) ) ;
#10283 = EDGE_LOOP ( 'NONE', ( #6688, #441, #77, #3620, #4167, #8585, #9774, #3220, #6721, #3768, #9840, #8522 ) ) ;
#10284 = CARTESIAN_POINT ( 'NONE',  ( 42.63976443033212860, 50.99948385550240459, 0.02388180880522514787 ) ) ;
#10285 = ORIENTED_EDGE ( 'NONE', *, *, #3742, .F. ) ;
#10286 = CARTESIAN_POINT ( 'NONE',  ( 4.086376210449952140, 2.103254844323300343, 3.500000000000000000 ) ) ;
#10287 = ORIENTED_EDGE ( 'NONE', *, *, #132, .F. ) ;
#10288 = LINE ( 'NONE', #727, #2984 ) ;
#10289 = CARTESIAN_POINT ( 'NONE',  ( 3.972709601346592123, -2.746729940827190575, 2.374099244652734697 ) ) ;
#10290 = CARTESIAN_POINT ( 'NONE',  ( 62.49999999999998579, 45.00000000000001421, 9.999999999999998224 ) ) ;
#10291 = VECTOR ( 'NONE', #7635, 1000.000000000000000 ) ;
#10292 = CARTESIAN_POINT ( 'NONE',  ( 50.02271294988506156, 58.50051614449765225, -6.000000000000000888 ) ) ;
#10293 = AXIS2_PLACEMENT_3D ( 'NONE', #4120, #5303, #9508 ) ;
#10294 = CARTESIAN_POINT ( 'NONE',  ( 53.50000000000000000, 0.000000000000000000, 3.309499999999999886 ) ) ;
#10295 = CARTESIAN_POINT ( 'NONE',  ( 56.79116909180255135, 59.79948385550240175, -4.963592699179005585 ) ) ;
#10296 = CARTESIAN_POINT ( 'NONE',  ( 50.02271294988512551, 62.49948385550240459, 7.000000000000000888 ) ) ;
#10297 = CARTESIAN_POINT ( 'NONE',  ( 0.000000000000000000, 0.000000000000000000, -5.000000000000000000 ) ) ;
#10298 = CARTESIAN_POINT ( 'NONE',  ( 49.97728705011486738, 49.49948385550241170, -8.000000000000001776 ) ) ;
#10299 = VERTEX_POINT ( 'NONE', #8662 ) ;
#10300 = EDGE_LOOP ( 'NONE', ( #2647, #6706, #11287, #2332, #9152 ) ) ;
#10301 = ORIENTED_EDGE ( 'NONE', *, *, #5444, .F. ) ;
#10302 = DIRECTION ( 'NONE',  ( -0.000000000000000000, -0.000000000000000000, 1.000000000000000000 ) ) ;
#10303 = VECTOR ( 'NONE', #11347, 1000.000000000000000 ) ;
#10304 =( LENGTH_UNIT ( ) NAMED_UNIT ( * ) SI_UNIT ( .MILLI., .METRE. ) );
#10305 = DIRECTION ( 'NONE',  ( 1.000000000000000000, 0.000000000000000000, 0.000000000000000000 ) ) ;
#10306 = DIRECTION ( 'NONE',  ( -0.04542589977017699732, 0.9989677110047501252, 0.000000000000000000 ) ) ;
#10307 = DIRECTION ( 'NONE',  ( 0.000000000000000000, 0.000000000000000000, 1.000000000000000000 ) ) ;
#10308 = CARTESIAN_POINT ( 'NONE',  ( 55.11794222512601493, 64.19948385550240744, 3.688883143319541702 ) ) ;
#10309 = CARTESIAN_POINT ( 'NONE',  ( 52.29715082351539479, 54.60051614449766788, -6.992620115222796251 ) ) ;
#10310 = EDGE_CURVE ( 'NONE', #12157, #3807, #7624, .T. ) ;
#10311 = CARTESIAN_POINT ( 'NONE',  ( 45.31609314410960820, 58.30051614449765651, -6.485486291978072693 ) ) ;
#10312 = CARTESIAN_POINT ( 'NONE',  ( 4.071447262713888016, -2.020725942163694722, -3.499999999999999556 ) ) ;
#10313 = CARTESIAN_POINT ( 'NONE',  ( 57.60143344285435774, 49.10051614449766788, 2.493737253992045044 ) ) ;
#10315 = ORIENTED_EDGE ( 'NONE', *, *, #8914, .F. ) ;
#10314 = EDGE_LOOP ( 'NONE', ( #2213, #5943, #10270, #5983 ) ) ;
#10316 = ORIENTED_EDGE ( 'NONE', *, *, #3320, .T. ) ;
#10317 = EDGE_LOOP ( 'NONE', ( #1632, #632, #79, #11445 ) ) ;
#10318 = EDGE_CURVE ( 'NONE', #11844, #10505, #3738, .T. ) ;
#10319 = CARTESIAN_POINT ( 'NONE',  ( -12.99038105676659427, -12.50000000000003020, -9.000000000000000000 ) ) ;
#10320 = EDGE_CURVE ( 'NONE', #11359, #245, #8103, .T. ) ;
#10321 = EDGE_CURVE ( 'NONE', #11056, #8472, #3810, .T. ) ;
#10322 = CARTESIAN_POINT ( 'NONE',  ( 1.925929944387235853E-31, 15.00000000000001599, -9.999999999999998224 ) ) ;
#10323 = CARTESIAN_POINT ( 'NONE',  ( 6.244297270354684848, -1.798312406574552930E-11, -5.105276777067894400 ) ) ;
#10324 = ADVANCED_FACE ( 'NONE', ( #12240 ), #1792, .T. ) ;
#10325 = SHAPE_DEFINITION_REPRESENTATION ( #7862, #7264 ) ;
#10326 = CARTESIAN_POINT ( 'NONE',  ( 44.05948171654949874, 62.79948385550241596, 4.345558710429105354 ) ) ;
#10327 = CARTESIAN_POINT ( 'NONE',  ( 47.70284917648453415, 61.39948385550241028, -6.992620115222774047 ) ) ;
#10328 = LINE ( 'NONE', #699, #10432 ) ;
#10329 = CARTESIAN_POINT ( 'NONE',  ( 2.899426713160750069, -23.82535289025860337, -8.999999999999996447 ) ) ;
#10330 = FACE_OUTER_BOUND ( 'NONE', #5653, .T. ) ;
#10331 = CARTESIAN_POINT ( 'NONE',  ( 52.29715082351538769, 50.60051614449766788, -6.992620115222796251 ) ) ;
#10332 = CARTESIAN_POINT ( 'NONE',  ( 53.50833635130540955, 55.69948385550240744, -4.867452303228209765 ) ) ;
#10333 = DIRECTION ( 'NONE',  ( -1.000000000000000000, -0.000000000000000000, -0.000000000000000000 ) ) ;
#10334 = ORIENTED_EDGE ( 'NONE', *, *, #5526, .T. ) ;
#10335 = DIRECTION ( 'NONE',  ( 0.000000000000000000, 0.000000000000000000, 1.000000000000000000 ) ) ;
#10336 = ORIENTED_EDGE ( 'NONE', *, *, #9656, .T. ) ;
#10337 = ORIENTED_EDGE ( 'NONE', *, *, #11945, .F. ) ;
#10338 = DIRECTION ( 'NONE',  ( 1.000000000000000000, 0.000000000000000000, 0.000000000000000000 ) ) ;
#10339 = VECTOR ( 'NONE', #1488, 1000.000000000000114 ) ;
#10340 = DIRECTION ( 'NONE',  ( 0.000000000000000000, 0.000000000000000000, 1.000000000000000000 ) ) ;
#10341 = CARTESIAN_POINT ( 'NONE',  ( 0.000000000000000000, 0.000000000000000000, -25.03750572909317285 ) ) ;
#10342 =( NAMED_UNIT ( * ) PLANE_ANGLE_UNIT ( ) SI_UNIT ( $, .RADIAN. ) );
#10343 = CARTESIAN_POINT ( 'NONE',  ( 52.29715082351547295, 46.39948385550240317, 6.992620115222774047 ) ) ;
#10344 = DIRECTION ( 'NONE',  ( 0.000000000000000000, -0.000000000000000000, 1.000000000000000000 ) ) ;
#10345 = CARTESIAN_POINT ( 'NONE',  ( 3.806834918298644954, -3.031088913245541416, -1.749999999999998890 ) ) ;
#10346 = CARTESIAN_POINT ( 'NONE',  ( 55.08986747509849380, 47.20051614449766220, 3.727524721679155384 ) ) ;
#10347 = DIRECTION ( 'NONE',  ( 1.000000000000000000, 0.000000000000000000, 0.000000000000000000 ) ) ;
#10348 = CARTESIAN_POINT ( 'NONE',  ( 44.03140696652192787, 57.19948385550238612, -4.306917132069425058 ) ) ;
#10349 = CARTESIAN_POINT ( 'NONE',  ( 56.66441430157296821, 56.09948385550240602, 2.141517661632100111 ) ) ;
#10350 = AXIS2_PLACEMENT_3D ( 'NONE', #4542, #3772, #4610 ) ;
#10351 = ORIENTED_EDGE ( 'NONE', *, *, #8566, .T. ) ;
#10352 = CARTESIAN_POINT ( 'NONE',  ( 47.70284917648453415, 49.39948385550238896, -6.992620115222774047 ) ) ;
#10353=STYLED_ITEM('',(#13712),#5714);
#10354 = ORIENTED_EDGE ( 'NONE', *, *, #11929, .T. ) ;
#10355 = CARTESIAN_POINT ( 'NONE',  ( 4.180231680468789790, -2.085385483809538698, 3.570466434508605680 ) ) ;
#10356 = ORIENTED_EDGE ( 'NONE', *, *, #194, .T. ) ;
#10357 = B_SPLINE_CURVE_WITH_KNOTS ( 'NONE', 3,
 ( #5355, #2089, #1105, #6463, #4238, #3063 ),
 .UNSPECIFIED., .F., .F.,
 ( 4, 2, 4 ),
 ( -3.640115492409406142E-06, 0.0002066546034006526487, 0.0004169493222937146744 ),
 .UNSPECIFIED. ) ;
#10358 = DIRECTION ( 'NONE',  ( 1.000000000000000000, 0.000000000000000000, 0.000000000000000000 ) ) ;
#10359 = EDGE_CURVE ( 'NONE', #9809, #3329, #540, .T. ) ;
#10360 = AXIS2_PLACEMENT_3D ( 'NONE', #296, #1791, #364 ) ;
#10361 = DIRECTION ( 'NONE',  ( 1.000000000000000000, 0.000000000000000000, 0.000000000000000000 ) ) ;
#10362 = CARTESIAN_POINT ( 'NONE',  ( 42.63976443033212149, 46.99948385550240459, 0.02388180880522514787 ) ) ;
#10363 = VECTOR ( 'NONE', #12883, 1000.000000000000000 ) ;
#10364 = CARTESIAN_POINT ( 'NONE',  ( 55.94051828345053679, 49.20051614449766930, 4.345558710429044069 ) ) ;
#10365 = AXIS2_PLACEMENT_3D ( 'NONE', #6212, #12676, #10335 ) ;
#10366 = CARTESIAN_POINT ( 'NONE',  ( 6.371506350351443082, -3.439339428956426747, 4.260454149911180544 ) ) ;
#10367 = CARTESIAN_POINT ( 'NONE',  ( 47.42335538002188144, 56.59948385550239891, 8.007379884777233059 ) ) ;
#10368 = LINE ( 'NONE', #6104, #8460 ) ;
#10369 = CARTESIAN_POINT ( 'NONE',  ( 56.79116909180255135, 51.79948385550240175, -4.963592699179005585 ) ) ;
#10370 = AXIS2_PLACEMENT_3D ( 'NONE', #204, #4426, #11957 ) ;
#10371 = ORIENTED_EDGE ( 'NONE', *, *, #2536, .T. ) ;
#10372 = ORIENTED_EDGE ( 'NONE', *, *, #8475, .T. ) ;
#10373 = VERTEX_POINT ( 'NONE', #13192 ) ;
#10374 = DIRECTION ( 'NONE',  ( -0.000000000000000000, -0.000000000000000000, 1.000000000000000000 ) ) ;
#10375 = PLANE ( 'NONE',  #13499 ) ;
#10376 = CARTESIAN_POINT ( 'NONE',  ( -0.6507732100473471171, 4.243078065514775510, -0.2236248678334823436 ) ) ;
#10377 = STYLED_ITEM ( 'NONE', ( #8481 ), #8826 ) ;
#10378 = CARTESIAN_POINT ( 'NONE',  ( 53.54508667620428497, 60.29948385550240175, 4.840751629271157874 ) ) ;
#10379 = CARTESIAN_POINT ( 'NONE',  ( 47.74827507625470702, 62.40051614449765793, -7.007379884777204637 ) ) ;
#10380 = CARTESIAN_POINT ( 'NONE',  ( 43.20883090819742023, 60.20051614449766220, -4.963592699178938972 ) ) ;
#10381 = FACE_OUTER_BOUND ( 'NONE', #10819, .T. ) ;
#10382 = CARTESIAN_POINT ( 'NONE',  ( 47.37792948025170858, 51.60051614449766788, 7.992620115222797139 ) ) ;
#10384 = ORIENTED_EDGE ( 'NONE', *, *, #3665, .T. ) ;
#10383 = ORIENTED_EDGE ( 'NONE', *, *, #8703, .F. ) ;
#10385 = COLOUR_RGB ( '',0.8941176470588234615, 0.8941176470588234615, 0.8941176470588234615 ) ;
#10386 = ORIENTED_EDGE ( 'NONE', *, *, #9581, .T. ) ;
#10387 = VERTEX_POINT ( 'NONE', #9208 ) ;
#10388 = CIRCLE ( 'NONE', #4425, 4.799999999999999822 ) ;
#10389 = ADVANCED_FACE ( 'NONE', ( #6995 ), #11272, .T. ) ;
#10390 = CARTESIAN_POINT ( 'NONE',  ( -6.259644161404862988E-16, -4.618802153517027165, -3.504271511726793076 ) ) ;
#10391 = DIRECTION ( 'NONE',  ( 1.000000000000000000, 0.000000000000000000, 0.000000000000000000 ) ) ;
#10392 = LINE ( 'NONE', #3062, #2974 ) ;
#10393 = DIRECTION ( 'NONE',  ( 1.000000000000000000, 0.000000000000000000, -0.000000000000000000 ) ) ;
#10394 = APPLICATION_PROTOCOL_DEFINITION ( 'draft international standard', 'automotive_design', 1998, #2124 ) ;
#10395 = CARTESIAN_POINT ( 'NONE',  ( 52.25172492374522903, 63.59948385550237759, -7.007379884777225953 ) ) ;
#10396 = CARTESIAN_POINT ( 'NONE',  ( 56.65037692655918988, 61.89948385550241028, -2.184720259617163762 ) ) ;
#10397 = CARTESIAN_POINT ( 'NONE',  ( 52.25172492374527877, 61.40051614449765083, 7.007379884777203749 ) ) ;
#10398 = AXIS2_PLACEMENT_3D ( 'NONE', #6795, #6663, #9962 ) ;
#10399 = LINE ( 'NONE', #9368, #10851 ) ;
#10400 = CARTESIAN_POINT ( 'NONE',  ( 0.000000000000000000, 0.000000000000000000, -5.000000000000000000 ) ) ;
#10401 = DIRECTION ( 'NONE',  ( 0.3420201433256622736, 0.000000000000000000, -0.9396926207859106484 ) ) ;
#10402 = CARTESIAN_POINT ( 'NONE',  ( 50.02271294988505446, 50.50051614449765935, -7.000000000000000888 ) ) ;
#10403 = CARTESIAN_POINT ( 'NONE',  ( 43.69122665457040000, 52.99948385550241170, 0.02388180880521036456 ) ) ;
#10404 = CARTESIAN_POINT ( 'NONE',  ( 0.000000000000000000, 0.000000000000000000, 0.000000000000000000 ) ) ;
#10405 = VERTEX_POINT ( 'NONE', #7331 ) ;
#10406 = PLANE ( 'NONE',  #10293 ) ;
#10407 = ORIENTED_EDGE ( 'NONE', *, *, #13564, .F. ) ;
#10408 = ORIENTED_EDGE ( 'NONE', *, *, #1220, .F. ) ;
#10409 = CARTESIAN_POINT ( 'NONE',  ( -20.00000000000000000, -19.99999999999999289, -10.79827876554711530 ) ) ;
#10410 = DIRECTION ( 'NONE',  ( 0.000000000000000000, 0.000000000000000000, -1.000000000000000000 ) ) ;
#10411 = CARTESIAN_POINT ( 'NONE',  ( 6.518095160331717430, -2.933089652807539416, 5.080260301817235202 ) ) ;
#10412 = DIRECTION ( 'NONE',  ( 0.000000000000000000, 0.000000000000000000, -1.000000000000000000 ) ) ;
#10413 = CARTESIAN_POINT ( 'NONE',  ( -4.688877333428353111, -21.02685410450703074, 9.999999999999998224 ) ) ;
#10414 = CARTESIAN_POINT ( 'NONE',  ( 44.88205777487401349, 45.80051614449766362, 3.688883143319584779 ) ) ;
#10415 = FACE_BOUND ( 'NONE', #2038, .T. ) ;
#10416 = DIRECTION ( 'NONE',  ( 0.000000000000000000, 0.000000000000000000, 1.000000000000000000 ) ) ;
#10417 = CARTESIAN_POINT ( 'NONE',  ( 55.96859303347804371, 52.19948385550240033, 4.306917132069425946 ) ) ;
#10418 = AXIS2_PLACEMENT_3D ( 'NONE', #84, #1038, #8527 ) ;
#10419 = COLOUR_RGB ( '',0.8941176470588234615, 0.8941176470588234615, 0.8941176470588234615 ) ;
#10420 = AXIS2_PLACEMENT_3D ( 'NONE', #4601, #8687, #2242 ) ;
#10421 = EDGE_LOOP ( 'NONE', ( #2541, #6752 ) ) ;
#10422 = ADVANCED_FACE ( 'NONE', ( #5827 ), #744, .F. ) ;
#10423 = CARTESIAN_POINT ( 'NONE',  ( 47.70284917648453415, 53.39948385550238186, -6.992620115222774047 ) ) ;
#10424 = EDGE_CURVE ( 'NONE', #5079, #11951, #12754, .T. ) ;
#10425 = VERTEX_POINT ( 'NONE', #4995 ) ;
#10426 = FACE_OUTER_BOUND ( 'NONE', #5602, .T. ) ;
#10427 = ORIENTED_EDGE ( 'NONE', *, *, #1328, .T. ) ;
#10428 = EDGE_CURVE ( 'NONE', #9622, #10987, #12173, .T. ) ;
#10429 = CARTESIAN_POINT ( 'NONE',  ( -6.259644161404860030E-16, -4.618802153517027165, -3.433295621305388234 ) ) ;
#10430 = VECTOR ( 'NONE', #8996, 1000.000000000000000 ) ;
#10431 = CARTESIAN_POINT ( 'NONE',  ( 5.100000000000002309, 0.000000000000000000, 0.000000000000000000 ) ) ;
#10432 = VECTOR ( 'NONE', #3899, 1000.000000000000000 ) ;
#10433 = CARTESIAN_POINT ( 'NONE',  ( 47.74827507625477807, 46.59948385550239180, 7.007379884777229506 ) ) ;
#10434 = CARTESIAN_POINT ( 'NONE',  ( 50.02271294988505446, 46.50051614449765935, -7.000000000000000888 ) ) ;
#10435 = CYLINDRICAL_SURFACE ( 'NONE', #12162, 8.099999999999999645 ) ;
#10436 = CARTESIAN_POINT ( 'NONE',  ( 45.27934281921075410, 63.29948385550240175, -6.458785618021043895 ) ) ;
#10437 = CARTESIAN_POINT ( 'NONE',  ( 2.449293598294706513E-15, -20.00000000000000000, -8.999999999999998224 ) ) ;
#10438 = DIRECTION ( 'NONE',  ( 0.000000000000000000, 0.000000000000000000, 1.000000000000000000 ) ) ;
#10439 = CARTESIAN_POINT ( 'NONE',  ( 49.97728705011486738, 59.49948385550240459, -8.000000000000001776 ) ) ;
#10440 = ORIENTED_EDGE ( 'NONE', *, *, #1875, .F. ) ;
#10441 = ORIENTED_EDGE ( 'NONE', *, *, #7102, .F. ) ;
#10442 = CARTESIAN_POINT ( 'NONE',  ( 54.89903213687075834, 44.74560054925188268, -5.000000000000007105 ) ) ;
#10443 = AXIS2_PLACEMENT_3D ( 'NONE', #7623, #11827, #4574 ) ;
#10444 =( LENGTH_UNIT ( ) NAMED_UNIT ( * ) SI_UNIT ( .MILLI., .METRE. ) );
#10445 = DIRECTION ( 'NONE',  ( 0.000000000000000000, -0.000000000000000000, 1.000000000000000000 ) ) ;
#10446 = DIRECTION ( 'NONE',  ( -9.858538378746663627E-23, 5.031452844637890958E-23, -1.000000000000000000 ) ) ;
#10447 = CARTESIAN_POINT ( 'NONE',  ( 6.244297270353404095, 0.9889575675955796230, -5.105276777067857097 ) ) ;
#10448 = CARTESIAN_POINT ( 'NONE',  ( 51.92680522751238925, 49.40051614449766504, 6.007379884777208190 ) ) ;
#10449 = CARTESIAN_POINT ( 'NONE',  ( 52.25172492374528588, 59.40051614449765793, 7.007379884777204637 ) ) ;
#10450 = CARTESIAN_POINT ( 'NONE',  ( 42.39856655714564226, 64.10051614449766078, -2.493737253992044156 ) ) ;
#10451 = CARTESIAN_POINT ( 'NONE',  ( 2.449293598294706513E-15, -20.00000000000000000, 15.00000000000000355 ) ) ;
#10452 = CARTESIAN_POINT ( 'NONE',  ( 58.41169779390614281, 47.00051614449766646, 0.02388180880515032231 ) ) ;
#10453 = ORIENTED_EDGE ( 'NONE', *, *, #8401, .T. ) ;
#10454 = EDGE_CURVE ( 'NONE', #10906, #6800, #1720, .T. ) ;
#10455 = EDGE_LOOP ( 'NONE', ( #5582, #392, #4487, #5961 ) ) ;
#10456 = VERTEX_POINT ( 'NONE', #6923 ) ;
#10457 = CARTESIAN_POINT ( 'NONE',  ( 0.3126073911696451990, -4.041451884327386779, -1.834154111220703958E-17 ) ) ;
#10458 = CARTESIAN_POINT ( 'NONE',  ( 6.527192678185834929, 2.941622124011056272, -5.095038975456026797 ) ) ;
#10459 = DIRECTION ( 'NONE',  ( -1.000000000000000000, 0.000000000000000000, -0.000000000000000000 ) ) ;
#10460 = CARTESIAN_POINT ( 'NONE',  ( 62.49999999999998579, 45.00000000000001421, 0.000000000000000000 ) ) ;
#10461 = CARTESIAN_POINT ( 'NONE',  ( 44.28664221472220675, 53.09948385550240602, -1.832500667257165317 ) ) ;
#10462 = CARTESIAN_POINT ( 'NONE',  ( 54.13287192849676188, 62.29948385550240886, 5.649768623646098220 ) ) ;
#10463 = CARTESIAN_POINT ( 'NONE',  ( 54.13287192849671214, 58.70051614449765509, -5.649768623646139964 ) ) ;
#10464 = DIRECTION ( 'NONE',  ( -1.000000000000000000, 0.000000000000000000, 0.000000000000000000 ) ) ;
#10465 = PRODUCT_DEFINITION ( 'UNKNOWN', '', #10800, #6123 ) ;
#10466 = DIRECTION ( 'NONE',  ( -1.000000000000000000, 1.224646799147352714E-16, 0.000000000000000000 ) ) ;
#10467 = DIRECTION ( 'NONE',  ( 0.000000000000000000, 0.000000000000000000, 1.000000000000000000 ) ) ;
#10468 = CARTESIAN_POINT ( 'NONE',  ( 45.90387839640208512, 52.30051614449766362, -5.676469297603124353 ) ) ;
#10469 = CARTESIAN_POINT ( 'NONE',  ( 46.45491332379572924, 57.29948385550240175, -4.840751629271157874 ) ) ;
#10470 = CARTESIAN_POINT ( 'NONE',  ( 4.000000000000000000, 0.000000000000000000, 0.000000000000000000 ) ) ;
#10471 = VECTOR ( 'NONE', #12601, 1000.000000000000000 ) ;
#10472 = VERTEX_POINT ( 'NONE', #11130 ) ;
#10473 = DIRECTION ( 'NONE',  ( 1.000000000000000000, 0.000000000000000000, 0.000000000000000000 ) ) ;
#10474 = ORIENTED_EDGE ( 'NONE', *, *, #11961, .F. ) ;
#10475 = CIRCLE ( 'NONE', #7400, 4.000000000000000000 ) ;
#10476 = VERTEX_POINT ( 'NONE', #1651 ) ;
#10477 = CARTESIAN_POINT ( 'NONE',  ( 6.436591462021355348, 2.894509378375960118, 5.013437306331775645 ) ) ;
#10478 = DIRECTION ( 'NONE',  ( -0.7071067811865533459, 8.659560562354861368E-17, -0.7071067811865416886 ) ) ;
#10479 = CIRCLE ( 'NONE', #11592, 0.4999999999999972244 ) ;
#10480 = FACE_OUTER_BOUND ( 'NONE', #4302, .T. ) ;
#10481 = LINE ( 'NONE', #1905, #12565 ) ;
#10482 = FACE_OUTER_BOUND ( 'NONE', #3755, .T. ) ;
#10483 = CARTESIAN_POINT ( 'NONE',  ( 55.71335778527780036, 52.90051614449766504, -1.832500667257213056 ) ) ;
#10484 = EDGE_CURVE ( 'NONE', #4781, #9119, #8171, .T. ) ;
#10485 = LINE ( 'NONE', #11534, #9392 ) ;
#10486 = AXIS2_PLACEMENT_3D ( 'NONE', #7034, #1836, #644 ) ;
#10487 = CARTESIAN_POINT ( 'NONE',  ( 50.02271294988512551, 62.49948385550240459, 7.000000000000000888 ) ) ;
#10488 = CARTESIAN_POINT ( 'NONE',  ( 55.96859303347804371, 58.19948385550241454, 4.306917132069425946 ) ) ;
#10489 = VERTEX_POINT ( 'NONE', #9136 ) ;
#10490 = B_SPLINE_CURVE_WITH_KNOTS ( 'NONE', 3,
 ( #12957, #509, #10960, #10890, #10055, #4749, #13096, #13227 ),
 .UNSPECIFIED., .F., .F.,
 ( 4, 2, 2, 4 ),
 ( 2.465131517071610173E-07, 0.001183067374689837636, 0.001774477805458902699, 0.002365888236227967761 ),
 .UNSPECIFIED. ) ;
#10491 = AXIS2_PLACEMENT_3D ( 'NONE', #8696, #1270, #4276 ) ;
#10492 = ORIENTED_EDGE ( 'NONE', *, *, #9317, .F. ) ;
#10493 = CARTESIAN_POINT ( 'NONE',  ( 4.175813232069148562, 4.122719923832741884, -2.765695189283172261E-17 ) ) ;
#10494 = ADVANCED_FACE ( 'NONE', ( #2840 ), #4925, .F. ) ;
#10495 = CARTESIAN_POINT ( 'NONE',  ( 4.142654963991853734, 2.035398498734346973, 3.525413613457309747 ) ) ;
#10496 = DIRECTION ( 'NONE',  ( 1.000000000000000000, 0.000000000000000000, 0.000000000000000000 ) ) ;
#10497 = ADVANCED_FACE ( 'NONE', ( #10092 ), #11059, .T. ) ;
#10498 = DIRECTION ( 'NONE',  ( -1.000000000000000000, 0.000000000000000000, 0.000000000000000000 ) ) ;
#10499 = CARTESIAN_POINT ( 'NONE',  ( 45.90387839640208512, 48.30051614449765651, -5.676469297603124353 ) ) ;
#10500 = EDGE_CURVE ( 'NONE', #7846, #10200, #6807, .T. ) ;
#10501 = CARTESIAN_POINT ( 'NONE',  ( 6.244889965166096957, -4.918546365148221078, 1.691415889817839746 ) ) ;
#10502 = CARTESIAN_POINT ( 'NONE',  ( 45.31609314410967926, 64.69948385550240744, 6.485486291978119766 ) ) ;
#10503 =( NAMED_UNIT ( * ) PLANE_ANGLE_UNIT ( ) SI_UNIT ( $, .RADIAN. ) );
#10504 = CARTESIAN_POINT ( 'NONE',  ( 52.57664461997811856, 55.59948385550240602, -8.007379884777229506 ) ) ;
#10505 = VERTEX_POINT ( 'NONE', #1579 ) ;
#10506 = VERTEX_POINT ( 'NONE', #10023 ) ;
#10507 = PLANE ( 'NONE',  #4845 ) ;
#10508 = VECTOR ( 'NONE', #8588, 1000.000000000000000 ) ;
#10509 = CARTESIAN_POINT ( 'NONE',  ( 0.5000000000000000000, -6.429618962271402616, 0.000000000000000000 ) ) ;
#10510 = EDGE_CURVE ( 'NONE', #11165, #2102, #4851, .T. ) ;
#10511 = CARTESIAN_POINT ( 'NONE',  ( 6.327632967270674591, -5.346704644969953790, 0.7392359018479527366 ) ) ;
#10512 = CARTESIAN_POINT ( 'NONE',  ( 22.00000000000000000, -20.00000000000000000, -20.00000000000000000 ) ) ;
#10513 = CARTESIAN_POINT ( 'NONE',  ( 46.45491332379576477, 47.70051614449766220, 4.840751629271188961 ) ) ;
#10514 = ADVANCED_FACE ( 'NONE', ( #12222 ), #1054, .F. ) ;
#10515 = CARTESIAN_POINT ( 'NONE',  ( 49.97728705011495265, 57.50051614449766646, 7.000000000000000888 ) ) ;
#10516 = CARTESIAN_POINT ( 'NONE',  ( 47.42335538002180328, 64.40051614449764372, -8.007379884777206414 ) ) ;
#10517 = CARTESIAN_POINT ( 'NONE',  ( 4.000000000000000000, 0.1981133338132474442, 2.382280164152719704E-17 ) ) ;
#10518 = CARTESIAN_POINT ( 'NONE',  ( 58.41169779390614281, 57.00051614449766646, 0.02388180880515032231 ) ) ;
#10519 = PRODUCT_DEFINITION_SHAPE ( 'NONE', 'NONE',  #13665 ) ;
#10520 = ORIENTED_EDGE ( 'NONE', *, *, #2758, .F. ) ;
#10521 = SHAPE_REPRESENTATION ( 'driver roller', ( #430 ), #13240 ) ;
#10522 = CIRCLE ( 'NONE', #3456, 12.50000000000000000 ) ;
#10523 = ORIENTED_EDGE ( 'NONE', *, *, #5326, .F. ) ;
#10524 = ORIENTED_EDGE ( 'NONE', *, *, #11339, .T. ) ;
#10525 = CARTESIAN_POINT ( 'NONE',  ( 6.403457969954082785, 5.776886471390908717, -1.402224347649779865E-18 ) ) ;
#10526 = DIRECTION ( 'NONE',  ( 1.000000000000000000, 3.469446951953615175E-16, 0.000000000000000000 ) ) ;
#10527 = CARTESIAN_POINT ( 'NONE',  ( 30.00000000000000000, -40.00000000000000000, 12.50000000000000000 ) ) ;
#10528 = LINE ( 'NONE', #9492, #3570 ) ;
#10529 = EDGE_CURVE ( 'NONE', #11112, #6155, #9676, .T. ) ;
#10530 = CARTESIAN_POINT ( 'NONE',  ( 48.07319477248768180, 48.59948385550239891, 6.007379884777225953 ) ) ;
#10531 = EDGE_CURVE ( 'NONE', #9171, #6905, #12086, .T. ) ;
#10532 = DIRECTION ( 'NONE',  ( 0.000000000000000000, 0.000000000000000000, -1.000000000000000000 ) ) ;
#10533 = CARTESIAN_POINT ( 'NONE',  ( 54.68390685589039890, 49.30051614449766362, 6.485486291978072693 ) ) ;
#10534 = FACE_OUTER_BOUND ( 'NONE', #7360, .T. ) ;
#10535 = DIRECTION ( 'NONE',  ( -3.469446951953611033E-15, 1.000000000000000000, 0.000000000000000000 ) ) ;
#10536 = DIRECTION ( 'NONE',  ( 0.1305261922200524616, 0.9914448613738103822, -0.000000000000000000 ) ) ;
#10537 = CARTESIAN_POINT ( 'NONE',  ( 56.66441430157294690, 54.90051614449765793, -2.141517661632166281 ) ) ;
#10538 = CARTESIAN_POINT ( 'NONE',  ( 56.30877334542961421, 59.99948385550241170, -0.02388180880520959434 ) ) ;
#10539 = CARTESIAN_POINT ( 'NONE',  ( -4.999999999999998224, -20.00000000000000000, 15.00000000000000355 ) ) ;
#10540 = ORIENTED_EDGE ( 'NONE', *, *, #4660, .T. ) ;
#10541 = FACE_OUTER_BOUND ( 'NONE', #2753, .T. ) ;
#10542 = VERTEX_POINT ( 'NONE', #8776 ) ;
#10543 = DIRECTION ( 'NONE',  ( -0.000000000000000000, -0.000000000000000000, -1.000000000000000000 ) ) ;
#10544 = FACE_BOUND ( 'NONE', #941, .T. ) ;
#10545 = LINE ( 'NONE', #5307, #666 ) ;
#10546 = SHAPE_REPRESENTATION_RELATIONSHIP ( 'NONE' , 'NONE' ,  #180, #8826 ) ;
#10547 = CARTESIAN_POINT ( 'NONE',  ( 57.36023556966787851, 49.99948385550238328, -0.02388180880522424582 ) ) ;
#10548 = CARTESIAN_POINT ( 'NONE',  ( 0.02448733951239481094, 4.877042772274728044, -3.751161874094022242 ) ) ;
#10549 = CARTESIAN_POINT ( 'NONE',  ( 46.49166364869456913, 52.30051614449766362, -4.867452303228181343 ) ) ;
#10550 = CARTESIAN_POINT ( 'NONE',  ( 2.449293598294706513E-15, -20.00000000000000000, -9.999999999999994671 ) ) ;
#10551 = CARTESIAN_POINT ( 'NONE',  ( 45.90387839640214196, 62.69948385550240744, 5.676469297603166098 ) ) ;
#10552 = CARTESIAN_POINT ( 'NONE',  ( 47.70284917648453415, 61.39948385550241738, -6.992620115222774047 ) ) ;
#10553 = CARTESIAN_POINT ( 'NONE',  ( 50.02271294988512551, 62.49948385550240459, 7.000000000000000888 ) ) ;
#10554 = EDGE_CURVE ( 'NONE', #5028, #8692, #1559, .T. ) ;
#10555 = ORIENTED_EDGE ( 'NONE', *, *, #9738, .T. ) ;
#10556 = ORIENTED_EDGE ( 'NONE', *, *, #1611, .T. ) ;
#10557 = CARTESIAN_POINT ( 'NONE',  ( 0.02511973781850649831, -4.877415612947427981, -3.751298745799844792 ) ) ;
#10558 = EDGE_CURVE ( 'NONE', #8238, #4274, #3941, .T. ) ;
#10559 = LINE ( 'NONE', #5518, #8731 ) ;
#10560 = DIRECTION ( 'NONE',  ( -0.6520673188974834833, 0.7581610723493046322, 1.805535875966852419E-17 ) ) ;
#10561 = CARTESIAN_POINT ( 'NONE',  ( 2.449293598294706513E-15, -20.00000000000000000, -20.00000000000000000 ) ) ;
#10562 = CARTESIAN_POINT ( 'NONE',  ( 45.60000000000000142, 2.789133085058097101E-16, -2.055000000000000160 ) ) ;
#10563 = CARTESIAN_POINT ( 'NONE',  ( 52.25172492374527877, 49.40051614449766504, 7.007379884777203749 ) ) ;
#10564 = AXIS2_PLACEMENT_3D ( 'NONE', #11111, #458, #522 ) ;
#10565 = FACE_OUTER_BOUND ( 'NONE', #11729, .T. ) ;
#10566 = CARTESIAN_POINT ( 'NONE',  ( 41.58830220609386430, 64.99948385550240459, 0.02388180880523263147 ) ) ;
#10567=STYLED_ITEM('',(#13719),#5785);
#10568 = DIRECTION ( 'NONE',  ( -0.000000000000000000, 1.000000000000000000, -0.000000000000000000 ) ) ;
#10569 = CARTESIAN_POINT ( 'NONE',  ( 43.18075615816989199, 57.19948385550241454, -4.924951120819313743 ) ) ;
#10570 = EDGE_CURVE ( 'NONE', #486, #8372, #10074, .T. ) ;
#10571 = ORIENTED_EDGE ( 'NONE', *, *, #4620, .T. ) ;
#10572 = EDGE_CURVE ( 'NONE', #5152, #9289, #4608, .T. ) ;
#10573 = ORIENTED_EDGE ( 'NONE', *, *, #10798, .F. ) ;
#10574 = CONICAL_SURFACE ( 'NONE', #8374, 8.105212085995399107, 1.221730476396037490 ) ;
#10575 = DIRECTION ( 'NONE',  ( 1.000000000000000000, 0.000000000000000000, 0.000000000000000000 ) ) ;
#10576 = CONICAL_SURFACE ( 'NONE', #3514, 4.000000000000003553, 1.029744260000001077 ) ;
#10577 = DIRECTION ( 'NONE',  ( -0.000000000000000000, 1.000000000000000000, 1.224646799147353207E-16 ) ) ;
#10578 = B_SPLINE_CURVE_WITH_KNOTS ( 'NONE', 3,
 ( #5524, #9109, #10062, #6898, #13372, #10135 ),
 .UNSPECIFIED., .F., .F.,
 ( 4, 2, 4 ),
 ( 0.01799235506992015107, 0.01945319861728521740, 0.02091404216465028373 ),
 .UNSPECIFIED. ) ;
#10579 = CARTESIAN_POINT ( 'NONE',  ( 6.244004651191001010, -4.663678638742299931, -2.132808149174403312 ) ) ;
#10580 = LINE ( 'NONE', #4094, #2337 ) ;
#10581 = CARTESIAN_POINT ( 'NONE',  ( 51.97223112728249816, 48.60051614449766788, -5.992620115222793586 ) ) ;
#10582 = CARTESIAN_POINT ( 'NONE',  ( 56.65037692655921120, 59.10051614449766078, 2.184720259617097593 ) ) ;
#10583 = MECHANICAL_DESIGN_GEOMETRIC_PRESENTATION_REPRESENTATION (  '', ( #8165 ), #855 ) ;
#10584 = CARTESIAN_POINT ( 'NONE',  ( 54.72065718078924590, 46.29948385550240886, 6.458785618021043895 ) ) ;
#10585 = CARTESIAN_POINT ( 'NONE',  ( 4.158413352280810216, -4.089743253945651524, 4.401844587977598791E-16 ) ) ;
#10586 = CARTESIAN_POINT ( 'NONE',  ( 54.68390685589039890, 53.30051614449767072, 6.485486291978072693 ) ) ;
#10587 = EDGE_LOOP ( 'NONE', ( #1081, #8728, #12972, #4321 ) ) ;
#10588 = EDGE_CURVE ( 'NONE', #7078, #9424, #11182, .T. ) ;
#10589 = ORIENTED_EDGE ( 'NONE', *, *, #7450, .T. ) ;
#10590 = ADVANCED_FACE ( 'NONE', ( #8917 ), #12973, .F. ) ;
#10591 = ORIENTED_EDGE ( 'NONE', *, *, #3246, .T. ) ;
#10592 = MECHANICAL_DESIGN_GEOMETRIC_PRESENTATION_REPRESENTATION (  '', ( #10377 ), #6626 ) ;
#10593 = CARTESIAN_POINT ( 'NONE',  ( 0.8816464618332836567, -24.71833652004169934, 9.999999999999998224 ) ) ;
#10595 = AXIS2_PLACEMENT_3D ( 'NONE', #3915, #13304, #10278 ) ;
#10594 = CARTESIAN_POINT ( 'NONE',  ( 6.367873360227556567, 2.886751345948123770, -5.000000000000000000 ) ) ;
#10596 = EDGE_CURVE ( 'NONE', #9119, #9043, #8977, .T. ) ;
#10597 = CARTESIAN_POINT ( 'NONE',  ( 62.49999999999998579, 20.00000000000001421, 15.00000000000000000 ) ) ;
#10598 = DIRECTION ( 'NONE',  ( 0.000000000000000000, 0.000000000000000000, 1.000000000000000000 ) ) ;
#10599 = PLANE ( 'NONE',  #2413 ) ;
#10600 = CARTESIAN_POINT ( 'NONE',  ( 43.69122665457040000, 48.99948385550241170, 0.02388180880521036456 ) ) ;
#10601 = CARTESIAN_POINT ( 'NONE',  ( 44.05948171654949874, 62.79948385550240886, 4.345558710429104465 ) ) ;
#10602 = CARTESIAN_POINT ( 'NONE',  ( 43.20883090819742023, 48.20051614449766930, -4.963592699178938972 ) ) ;
#10603 = CARTESIAN_POINT ( 'NONE',  ( -4.999999999999998224, -20.00000000000000000, 9.000000000000000000 ) ) ;
#10604 = LINE ( 'NONE', #226, #7573 ) ;
#10605 = CARTESIAN_POINT ( 'NONE',  ( 44.03140696652198471, 59.80051614449766362, 4.306917132069485454 ) ) ;
#10606 = CARTESIAN_POINT ( 'NONE',  ( 44.28664221472220675, 61.09948385550241312, -1.832500667257165317 ) ) ;
#10607 = AXIS2_PLACEMENT_3D ( 'NONE', #239, #9647, #8750 ) ;
#10608 = CARTESIAN_POINT ( 'NONE',  ( -22.14999999999999858, -19.99999999999999289, -23.00000000000000000 ) ) ;
#10609 = EDGE_LOOP ( 'NONE', ( #9185, #6160, #3253, #8453 ) ) ;
#10610 = CARTESIAN_POINT ( 'NONE',  ( 1.925929944387235853E-31, 15.00000000000001599, -9.000000000000001776 ) ) ;
#10611 = ORIENTED_EDGE ( 'NONE', *, *, #10531, .F. ) ;
#10612 = CARTESIAN_POINT ( 'NONE',  ( 6.420058897733091463, 2.891482565094592339, 5.008194711943422028 ) ) ;
#10613 = APPLICATION_CONTEXT ( 'automotive_design' ) ;
#10614 = FACE_OUTER_BOUND ( 'NONE', #6848, .T. ) ;
#10615 = CARTESIAN_POINT ( 'NONE',  ( 20.00000000000000000, -25.00000000000000711, -23.00000000000000000 ) ) ;
#10616 = CARTESIAN_POINT ( 'NONE',  ( 0.000000000000000000, 0.000000000000000000, 0.000000000000000000 ) ) ;
#10617 = CARTESIAN_POINT ( 'NONE',  ( 47.70284917648453415, 49.39948385550238896, -6.992620115222774047 ) ) ;
#10618 = VECTOR ( 'NONE', #13333, 1000.000000000000000 ) ;
#10619 = DIRECTION ( 'NONE',  ( 0.000000000000000000, 0.000000000000000000, 1.000000000000000000 ) ) ;
#10620 = CARTESIAN_POINT ( 'NONE',  ( 55.11794222512599362, 52.80051614449766362, -3.688883143319583446 ) ) ;
#10621 = CARTESIAN_POINT ( 'NONE',  ( 2.449293598294706513E-15, -20.00000000000000000, 15.00000000000000355 ) ) ;
#10622 = CARTESIAN_POINT ( 'NONE',  ( 45.90387839640214196, 64.69948385550240744, 5.676469297603166098 ) ) ;
#10623 = SURFACE_STYLE_FILL_AREA ( #306 ) ;
#10624 = CARTESIAN_POINT ( 'NONE',  ( 44.03140696652192787, 57.19948385550238612, -4.306917132069425058 ) ) ;
#10625 = ORIENTED_EDGE ( 'NONE', *, *, #13588, .T. ) ;
#10626 = CIRCLE ( 'NONE', #7335, 5.000000000000007994 ) ;
#10627 = VERTEX_POINT ( 'NONE', #581 ) ;
#10628 = VERTEX_POINT ( 'NONE', #4830 ) ;
#10629 = CARTESIAN_POINT ( 'NONE',  ( -3.540020015735593439, -2.810662092924100630, -3.602146406945814672 ) ) ;
#10630 = FACE_OUTER_BOUND ( 'NONE', #7791, .T. ) ;
#10631 = DIRECTION ( 'NONE',  ( 0.000000000000000000, 0.000000000000000000, -1.000000000000000000 ) ) ;
#10632 = PLANE ( 'NONE',  #1862 ) ;
#10633 = CARTESIAN_POINT ( 'NONE',  ( 45.90387839640214196, 50.69948385550240744, 5.676469297603166098 ) ) ;
#10634 = VECTOR ( 'NONE', #4718, 1000.000000000000000 ) ;
#10635 = CARTESIAN_POINT ( 'NONE',  ( 54.09612160359792199, 47.30051614449765651, 5.676469297603124353 ) ) ;
#10636 = EDGE_CURVE ( 'NONE', #13379, #4847, #597, .T. ) ;
#10637 = PRODUCT_DEFINITION_SHAPE ( 'NONE', 'NONE',  #13670 ) ;
#10638 = CARTESIAN_POINT ( 'NONE',  ( 45.15499999999999403, 3.061616997868383634E-16, -2.500000000000000444 ) ) ;
#10639 = CIRCLE ( 'NONE', #4242, 2.000000000000000888 ) ;
#10640 = CARTESIAN_POINT ( 'NONE',  ( 54.09612160359786515, 45.69948385550240744, -5.676469297603166098 ) ) ;
#10641 = FACE_OUTER_BOUND ( 'NONE', #6298, .T. ) ;
#10642 = PRODUCT_DEFINITION ( 'UNKNOWN', '', #4194, #8186 ) ;
#10643 = CARTESIAN_POINT ( 'NONE',  ( 50.02271294988513972, 58.49948385550241170, 8.000000000000001776 ) ) ;
#10644 = ORIENTED_EDGE ( 'NONE', *, *, #2561, .F. ) ;
#10645 = VECTOR ( 'NONE', #5064, 1000.000000000000000 ) ;
#10646 = ORIENTED_EDGE ( 'NONE', *, *, #5049, .T. ) ;
#10647 = DIRECTION ( 'NONE',  ( 1.000000000000000000, 0.000000000000000000, 0.000000000000000000 ) ) ;
#10648 = CARTESIAN_POINT ( 'NONE',  ( -4.799999999999999822, 5.878304635907294211E-16, -1.000000000000000000 ) ) ;
#10649 = DIRECTION ( 'NONE',  ( -0.000000000000000000, -0.000000000000000000, -1.000000000000000000 ) ) ;
#10650 = CARTESIAN_POINT ( 'NONE',  ( 44.91013252490150620, 48.20051614449766930, -3.727524721679154940 ) ) ;
#10651 = CARTESIAN_POINT ( 'NONE',  ( 45.86712807150329496, 57.70051614449765509, 5.649768623646139964 ) ) ;
#10652 = CARTESIAN_POINT ( 'NONE',  ( 41.58830220609386430, 46.99948385550239749, 0.02388180880523263147 ) ) ;
#10653 = AXIS2_PLACEMENT_3D ( 'NONE', #5138, #4092, #3706 ) ;
#10654 = LINE ( 'NONE', #5542, #7794 ) ;
#10655 = CARTESIAN_POINT ( 'NONE',  ( 41.58830220609386430, 56.00051614449765935, -0.02388180880514929535 ) ) ;
#10656 = VECTOR ( 'NONE', #10034, 1000.000000000000000 ) ;
#10658 = EDGE_CURVE ( 'NONE', #3147, #4780, #13114, .T. ) ;
#10657 = EDGE_LOOP ( 'NONE', ( #11969, #459, #10555 ) ) ;
#10659 = ORIENTED_EDGE ( 'NONE', *, *, #4827, .F. ) ;
#10660 = EDGE_LOOP ( 'NONE', ( #12855, #5600, #13553 ) ) ;
#10661 = PLANE ( 'NONE',  #2053 ) ;
#10662 = CARTESIAN_POINT ( 'NONE',  ( 6.481779955677444249, 2.910222513313288850, -5.040653254389421356 ) ) ;
#10663 = EDGE_CURVE ( 'NONE', #10425, #1787, #7696, .T. ) ;
#10664 = CARTESIAN_POINT ( 'NONE',  ( 4.197393957002303999, 7.772902908466098641E-14, -3.503767560748929810 ) ) ;
#10665 = DIRECTION ( 'NONE',  ( -0.8571673013836855759, 0.000000000000000000, -0.5150380737757258576 ) ) ;
#10666 = SURFACE_STYLE_FILL_AREA ( #2220 ) ;
#10667 = AXIS2_PLACEMENT_3D ( 'NONE', #8856, #12166, #7890 ) ;
#10668 = CARTESIAN_POINT ( 'NONE',  ( 44.91013252490152752, 50.79948385550240175, 3.727524721679198461 ) ) ;
#10669 = CARTESIAN_POINT ( 'NONE',  ( 3.973110223768738791, 0.6864646529411682074, 3.565797985667475967 ) ) ;
#10670 = ADVANCED_FACE ( 'NONE', ( #3655 ), #9328, .F. ) ;
#10671 = CARTESIAN_POINT ( 'NONE',  ( 50.02271294988505446, 44.50051614449765935, -8.000000000000001776 ) ) ;
#10672 = ADVANCED_FACE ( 'NONE', ( #2055 ), #4904, .F. ) ;
#10673 = DIRECTION ( 'NONE',  ( -0.000000000000000000, -0.000000000000000000, -1.000000000000000000 ) ) ;
#10674 = DIRECTION ( 'NONE',  ( 1.000000000000000000, 0.000000000000000000, 0.000000000000000000 ) ) ;
#10675 = CARTESIAN_POINT ( 'NONE',  ( 47.70284917648459100, 57.60051614449764656, 6.992620115222796251 ) ) ;
#10676 = CARTESIAN_POINT ( 'NONE',  ( 53.54508667620428497, 58.29948385550240886, 4.840751629271157874 ) ) ;
#10677 = DIRECTION ( 'NONE',  ( -0.000000000000000000, -0.000000000000000000, 1.000000000000000000 ) ) ;
#10678 = ORIENTED_EDGE ( 'NONE', *, *, #13522, .T. ) ;
#10679 = CARTESIAN_POINT ( 'NONE',  ( 1.567478505476135000E-15, 4.618802153517012954, -3.504269196027527844 ) ) ;
#10680 = EDGE_LOOP ( 'NONE', ( #10971, #4101, #9218 ) ) ;
#10681 = FACE_OUTER_BOUND ( 'NONE', #3993, .T. ) ;
#10682 = LINE ( 'NONE', #10745, #2505 ) ;
#10683 = DIRECTION ( 'NONE',  ( 0.000000000000000000, 0.000000000000000000, 1.000000000000000000 ) ) ;
#10684 =( NAMED_UNIT ( * ) SI_UNIT ( $, .STERADIAN. ) SOLID_ANGLE_UNIT ( ) );
#10685 = CARTESIAN_POINT ( 'NONE',  ( 45.90387839640214196, 52.69948385550240033, 5.676469297603166098 ) ) ;
#10686 = CARTESIAN_POINT ( 'NONE',  ( 0.000000000000000000, 3.031088913245533423, -1.750000000000004885 ) ) ;
#10687 = CARTESIAN_POINT ( 'NONE',  ( 49.97728705011494554, 51.50051614449765935, 6.000000000000000888 ) ) ;
#10688 = AXIS2_PLACEMENT_3D ( 'NONE', #7380, #1123, #11650 ) ;
#10689 = FACE_OUTER_BOUND ( 'NONE', #8085, .T. ) ;
#10690 = CARTESIAN_POINT ( 'NONE',  ( 6.244004651191001010, 4.663678638742294602, 2.132808149174402867 ) ) ;
#10691 = FILL_AREA_STYLE_COLOUR ( '', #11001 ) ;
#10692 = CARTESIAN_POINT ( 'NONE',  ( 57.36023556966787851, 59.99948385550240459, -0.02388180880522424582 ) ) ;
#10693 = CARTESIAN_POINT ( 'NONE',  ( 30.00000000000000000, 5.000000000000010658, 0.000000000000000000 ) ) ;
#10694 = ORIENTED_EDGE ( 'NONE', *, *, #4439, .F. ) ;
#10695 = ORIENTED_EDGE ( 'NONE', *, *, #11603, .T. ) ;
#10696 = EDGE_CURVE ( 'NONE', #967, #7922, #12360, .T. ) ;
#10697 = VERTEX_POINT ( 'NONE', #3998 ) ;
#10698 = CARTESIAN_POINT ( 'NONE',  ( 4.093692494532771953, 4.043567292011543302, -5.737475420082528345E-17 ) ) ;
#10699 = VECTOR ( 'NONE', #424, 1000.000000000000114 ) ;
#10700 = CARTESIAN_POINT ( 'NONE',  ( 2.449293598294706513E-15, -5.000000000000000888, -9.000000000000000000 ) ) ;
#10701 = CARTESIAN_POINT ( 'NONE',  ( -2.855764796983342624, 2.970025579236414082, -0.09382832055445475272 ) ) ;
#10702 = CYLINDRICAL_SURFACE ( 'NONE', #3195, 5.000000000000000000 ) ;
#10703 = CARTESIAN_POINT ( 'NONE',  ( 45.86712807150323812, 55.29948385550240175, -5.649768623646098220 ) ) ;
#10704 = VECTOR ( 'NONE', #6751, 1000.000000000000000 ) ;
#10705 = CARTESIAN_POINT ( 'NONE',  ( 52.29715082351538769, 52.60051614449766788, -6.992620115222796251 ) ) ;
#10706 = CARTESIAN_POINT ( 'NONE',  ( -14.14213562373094746, -25.00000000000000000, -23.00000000000000000 ) ) ;
#10707 = CARTESIAN_POINT ( 'NONE',  ( 58.41169779390614281, 63.99948385550241170, -0.02388180880523160798 ) ) ;
#10708 = SURFACE_STYLE_FILL_AREA ( #5527 ) ;
#10709 = VECTOR ( 'NONE', #8512, 1000.000000000000114 ) ;
#10710 = CARTESIAN_POINT ( 'NONE',  ( 41.58830220609386430, 56.99948385550241170, 0.02388180880523263147 ) ) ;
#10711 = ORIENTED_EDGE ( 'NONE', *, *, #7251, .F. ) ;
#10712 = ORIENTED_EDGE ( 'NONE', *, *, #9059, .T. ) ;
#10713 = DIRECTION ( 'NONE',  ( -0.000000000000000000, -0.000000000000000000, 1.000000000000000000 ) ) ;
#10714 = LINE ( 'NONE', #4560, #7321 ) ;
#10715 = CARTESIAN_POINT ( 'NONE',  ( 48.07319477248762496, 50.40051614449766504, -6.007379884777208190 ) ) ;
#10716 = DIRECTION ( 'NONE',  ( 0.000000000000000000, 0.000000000000000000, 1.000000000000000000 ) ) ;
#10717 = CARTESIAN_POINT ( 'NONE',  ( 58.41169779390614281, 45.99948385550240459, -0.02388180880523160798 ) ) ;
#10718 = DIRECTION ( 'NONE',  ( -1.000000000000000000, 0.000000000000000000, 0.000000000000000000 ) ) ;
#10719 = CARTESIAN_POINT ( 'NONE',  ( 47.42335538002180328, 56.40051614449765793, -8.007379884777206414 ) ) ;
#10720 = ORIENTED_EDGE ( 'NONE', *, *, #8047, .F. ) ;
#10721 = EDGE_LOOP ( 'NONE', ( #10573, #1807, #937 ) ) ;
#10722 = EDGE_LOOP ( 'NONE', ( #3383, #4364, #9983, #8640, #1926, #1969, #5317, #7672, #7990, #1249, #4591, #11797, #12317, #12320, #11379, #2503, #3483, #9252, #12872, #3317, #8389, #10659, #4795, #11444, #8846, #13004, #6642, #4497, #2345 ) ) ;
#10723 = VERTEX_POINT ( 'NONE', #7113 ) ;
#10724 = DIRECTION ( 'NONE',  ( -0.9768494444668812671, -0.2139279384389642935, 0.000000000000000000 ) ) ;
#10725 = ADVANCED_FACE ( 'NONE', ( #10218 ), #2167, .T. ) ;
#10726 = CARTESIAN_POINT ( 'NONE',  ( -2.649999999999988365, 15.00000000000001599, 15.00000000000000000 ) ) ;
#10727 = DIRECTION ( 'NONE',  ( 1.000000000000000000, 0.000000000000000000, 0.000000000000000000 ) ) ;
#10728 = CARTESIAN_POINT ( 'NONE',  ( 2.449293598294706513E-15, -20.00000000000000000, 9.000000000000000000 ) ) ;
#10729 = CARTESIAN_POINT ( 'NONE',  ( 44.88205777487398507, 51.19948385550240744, -3.688883143319540814 ) ) ;
#10730 = CARTESIAN_POINT ( 'NONE',  ( 47.70284917648453415, 65.39948385550239607, -6.992620115222774047 ) ) ;
#10731 = CARTESIAN_POINT ( 'NONE',  ( 58.41169779390614281, 47.00051614449766646, 0.02388180880515032231 ) ) ;
#10732 = AXIS2_PLACEMENT_3D ( 'NONE', #6340, #12399, #11580 ) ;
#10733 = FACE_OUTER_BOUND ( 'NONE', #7095, .T. ) ;
#10734 = DIRECTION ( 'NONE',  ( 0.5000000000000013323, -0.8660254037844379305, 0.000000000000000000 ) ) ;
#10735 = CARTESIAN_POINT ( 'NONE',  ( 45.90387839640208512, 56.30051614449765651, -5.676469297603124353 ) ) ;
#10736 = CARTESIAN_POINT ( 'NONE',  ( 56.30877334542961421, 55.99948385550241170, -0.02388180880520959434 ) ) ;
#10737 = EDGE_CURVE ( 'NONE', #504, #12170, #11667, .T. ) ;
#10738 = EDGE_LOOP ( 'NONE', ( #3653, #12191, #4340, #10440, #4939 ) ) ;
#10739 = LINE ( 'NONE', #165, #3084 ) ;
#10740 = EDGE_CURVE ( 'NONE', #6155, #3623, #6235, .T. ) ;
#10741 = ORIENTED_EDGE ( 'NONE', *, *, #8841, .T. ) ;
#10742 = CARTESIAN_POINT ( 'NONE',  ( -8.759913291900485177, -7.823632761846201156, -9.000000000000000000 ) ) ;
#10743 = EDGE_CURVE ( 'NONE', #4149, #720, #9898, .T. ) ;
#10744 = PRODUCT_DEFINITION_SHAPE ( 'NONE', 'NONE',  #4727 ) ;
#10745 = CARTESIAN_POINT ( 'NONE',  ( -31.74999999999995737, 4.286263797015736595E-16, -3.500000000000000000 ) ) ;
#10746 = DIRECTION ( 'NONE',  ( -9.710251638871371392E-17, -5.969973981896233748E-17, -1.000000000000000000 ) ) ;
#10747 =( NAMED_UNIT ( * ) PLANE_ANGLE_UNIT ( ) SI_UNIT ( $, .RADIAN. ) );
#10748 = CARTESIAN_POINT ( 'NONE',  ( 43.33558569842703179, 49.09948385550240602, -2.141517661632099223 ) ) ;
#10749 = CARTESIAN_POINT ( 'NONE',  ( 50.00000000000000000, 40.00000000000000000, -4.000000000000003553 ) ) ;
#10750 = CARTESIAN_POINT ( 'NONE',  ( 55.11794222512599362, 50.80051614449766362, -3.688883143319583446 ) ) ;
#10751 = DIRECTION ( 'NONE',  ( -0.7779254092217071648, -0.6283566325640553840, 1.130512422757410748E-16 ) ) ;
#10752 = CARTESIAN_POINT ( 'NONE',  ( -74.99999999999997158, 45.00000000000001421, 15.00000000000000000 ) ) ;
#10753 = CARTESIAN_POINT ( 'NONE',  ( 0.000000000000000000, 3.031088913245533867, 1.750000000000002887 ) ) ;
#10754 = CARTESIAN_POINT ( 'NONE',  ( 52.25172492374522903, 57.59948385550241312, -7.007379884777225953 ) ) ;
#10755 = DIRECTION ( 'NONE',  ( 1.000000000000000000, 0.000000000000000000, -0.000000000000000000 ) ) ;
#10756 = ORIENTED_EDGE ( 'NONE', *, *, #1946, .F. ) ;
#10757 = ORIENTED_EDGE ( 'NONE', *, *, #832, .T. ) ;
#10758 = CARTESIAN_POINT ( 'NONE',  ( 75.00000000000000000, 32.50000000000001421, -15.00000000000000000 ) ) ;
#10759 = FACE_OUTER_BOUND ( 'NONE', #11181, .T. ) ;
#10760 = DIRECTION ( 'NONE',  ( 1.000000000000000000, 0.000000000000000000, 0.000000000000000000 ) ) ;
#10761 = SURFACE_SIDE_STYLE ('',( #8765 ) ) ;
#10762 = FACE_BOUND ( 'NONE', #12024, .T. ) ;
#10763 = CARTESIAN_POINT ( 'NONE',  ( 49.97728705011488159, 53.49948385550240459, -7.000000000000000888 ) ) ;
#10764 = CARTESIAN_POINT ( 'NONE',  ( 47.74827507625469281, 54.40051614449766504, -7.007379884777203749 ) ) ;
#10765 = DIRECTION ( 'NONE',  ( -1.000000000000000000, 0.000000000000000000, -0.000000000000000000 ) ) ;
#10766 = CARTESIAN_POINT ( 'NONE',  ( 44.05948171654949874, 54.79948385550241596, 4.345558710429105354 ) ) ;
#10767 = VECTOR ( 'NONE', #12106, 1000.000000000000000 ) ;
#10768 = CARTESIAN_POINT ( 'NONE',  ( 57.61547081786812896, 64.09948385550239891, 2.450534656007040901 ) ) ;
#10769 = ORIENTED_EDGE ( 'NONE', *, *, #4834, .T. ) ;
#10770 = ADVANCED_FACE ( 'NONE', ( #1987 ), #13312, .F. ) ;
#10771 = EDGE_LOOP ( 'NONE', ( #3042, #2873 ) ) ;
#10772 = DIRECTION ( 'NONE',  ( 9.858538378746663627E-23, -5.031452844637890958E-23, 1.000000000000000000 ) ) ;
#10773 = AXIS2_PLACEMENT_3D ( 'NONE', #3169, #11661, #5392 ) ;
#10774 = DIRECTION ( 'NONE',  ( -0.000000000000000000, -0.000000000000000000, 1.000000000000000000 ) ) ;
#10775 = CARTESIAN_POINT ( 'NONE',  ( 51.97223112728249816, 52.60051614449765367, -5.992620115222793586 ) ) ;
#10776 = DIRECTION ( 'NONE',  ( -0.000000000000000000, -0.000000000000000000, -1.000000000000000000 ) ) ;
#10777 = CARTESIAN_POINT ( 'NONE',  ( 43.18075615816989199, 55.19948385550240744, -4.924951120819313743 ) ) ;
#10778 = CARTESIAN_POINT ( 'NONE',  ( 55.94051828345050836, 55.79948385550238044, -4.345558710429104465 ) ) ;
#10779 = PLANE ( 'NONE',  #11554 ) ;
#10780 = CARTESIAN_POINT ( 'NONE',  ( 50.02271294988505446, 54.50051614449765935, -8.000000000000001776 ) ) ;
#10781 = VECTOR ( 'NONE', #10941, 1000.000000000000000 ) ;
#10782 = ORIENTED_EDGE ( 'NONE', *, *, #1693, .F. ) ;
#10783 = ORIENTED_EDGE ( 'NONE', *, *, #3692, .F. ) ;
#10784 = ORIENTED_EDGE ( 'NONE', *, *, #5228, .F. ) ;
#10785 = ORIENTED_EDGE ( 'NONE', *, *, #7030, .T. ) ;
#10786 = FACE_OUTER_BOUND ( 'NONE', #10984, .T. ) ;
#10787 = CARTESIAN_POINT ( 'NONE',  ( 4.000000000000000000, 2.309401076758497151, -5.000000000000000000 ) ) ;
#10788 = FACE_OUTER_BOUND ( 'NONE', #4537, .T. ) ;
#10789 = CARTESIAN_POINT ( 'NONE',  ( 51.92680522751233951, 57.59948385550240602, -6.007379884777223289 ) ) ;
#10790 = AXIS2_PLACEMENT_3D ( 'NONE', #12439, #10374, #3114 ) ;
#10791 = CARTESIAN_POINT ( 'NONE',  ( 44.05948171654945611, 48.20051614449764799, -4.345558710429044069 ) ) ;
#10792 = CARTESIAN_POINT ( 'NONE',  ( 49.97728705011495265, 49.50051614449766646, 8.000000000000001776 ) ) ;
#10793 = ADVANCED_FACE ( 'NONE', ( #10426 ), #12455, .F. ) ;
#10794 = DIRECTION ( 'NONE',  ( -1.000000000000000000, -4.082155997157843695E-16, 0.000000000000000000 ) ) ;
#10795 = FACE_OUTER_BOUND ( 'NONE', #7894, .T. ) ;
#10796 = CARTESIAN_POINT ( 'NONE',  ( 54.09612160359792199, 59.30051614449766362, 5.676469297603124353 ) ) ;
#10797 = CARTESIAN_POINT ( 'NONE',  ( 44.91013252490152752, 62.79948385550240175, 3.727524721679198461 ) ) ;
#10798 = EDGE_CURVE ( 'NONE', #9705, #9468, #797, .T. ) ;
#10799 = ORIENTED_EDGE ( 'NONE', *, *, #11947, .T. ) ;
#10800 = PRODUCT_DEFINITION_FORMATION_WITH_SPECIFIED_SOURCE ( 'ANY', '', #2235, .NOT_KNOWN. ) ;
#10801 = AXIS2_PLACEMENT_3D ( 'NONE', #4006, #11187, #1637 ) ;
#10802 = CARTESIAN_POINT ( 'NONE',  ( 20.00000000000000000, -20.00000000000000000, -12.00000000000000000 ) ) ;
#10803 = ORIENTED_EDGE ( 'NONE', *, *, #2641, .T. ) ;
#10804 = CARTESIAN_POINT ( 'NONE',  ( -1.391697335622809950, -4.043246145443391448, -3.503898532754372575 ) ) ;
#10805 = AXIS2_PLACEMENT_3D ( 'NONE', #13204, #5772, #5838 ) ;
#10806 = LINE ( 'NONE', #6351, #8485 ) ;
#10807 = CARTESIAN_POINT ( 'NONE',  ( 6.541334450618642826, 2.987059910623326875, 5.112749838330405083 ) ) ;
#10808 = CARTESIAN_POINT ( 'NONE',  ( 52.29715082351547295, 50.39948385550240317, 6.992620115222774047 ) ) ;
#10809 = CIRCLE ( 'NONE', #1526, 4.799999999999999822 ) ;
#10810 = PLANE ( 'NONE',  #3981 ) ;
#10811 = CARTESIAN_POINT ( 'NONE',  ( 51.92680522751238925, 59.40051614449765793, 6.007379884777208190 ) ) ;
#10812 = CARTESIAN_POINT ( 'NONE',  ( -74.99999999999997158, -7.500000000000027534, 10.00000000000000000 ) ) ;
#10813 = CARTESIAN_POINT ( 'NONE',  ( 2.000000000000000000, -0.8865213383406694847, 1.535500000000001419 ) ) ;
#10814 = DIRECTION ( 'NONE',  ( 0.000000000000000000, 0.000000000000000000, -1.000000000000000000 ) ) ;
#10815 = CARTESIAN_POINT ( 'NONE',  ( 44.91013252490152752, 46.79948385550240886, 3.727524721679198461 ) ) ;
#10816 = CARTESIAN_POINT ( 'NONE',  ( 4.000000000000000000, -2.309401076758514915, -3.433295621305383349 ) ) ;
#10817 = VERTEX_POINT ( 'NONE', #12567 ) ;
#10818 = EDGE_CURVE ( 'NONE', #1542, #1878, #8365, .T. ) ;
#10819 = EDGE_LOOP ( 'NONE', ( #596, #12105, #11, #8932, #13191 ) ) ;
#10820 = CARTESIAN_POINT ( 'NONE',  ( 62.50000000000000000, 32.50000000000001421, -9.999999999999998224 ) ) ;
#10821 =( GEOMETRIC_REPRESENTATION_CONTEXT ( 3 ) GLOBAL_UNCERTAINTY_ASSIGNED_CONTEXT ( ( #13092 ) ) GLOBAL_UNIT_ASSIGNED_CONTEXT ( ( #10859, #8793, #5551 ) ) REPRESENTATION_CONTEXT ( 'NONE', 'WORKASPACE' ) );
#10822 = AXIS2_PLACEMENT_3D ( 'NONE', #542, #7964, #6997 ) ;
#10823 = DIRECTION ( 'NONE',  ( 0.000000000000000000, 0.000000000000000000, -1.000000000000000000 ) ) ;
#10824 = DIRECTION ( 'NONE',  ( -1.000000000000000000, -0.000000000000000000, -0.000000000000000000 ) ) ;
#10825 =( LENGTH_UNIT ( ) NAMED_UNIT ( * ) SI_UNIT ( .MILLI., .METRE. ) );
#10826 = DIRECTION ( 'NONE',  ( -0.000000000000000000, -0.000000000000000000, -1.000000000000000000 ) ) ;
#10827 = CARTESIAN_POINT ( 'NONE',  ( 3.999999999999999112, 2.309401076758497595, -3.504271511726784194 ) ) ;
#10828 = CARTESIAN_POINT ( 'NONE',  ( 42.63976443033212149, 50.99948385550240459, 0.02388180880522514787 ) ) ;
#10829 = CARTESIAN_POINT ( 'NONE',  ( 54.13287192849671214, 50.70051614449766220, -5.649768623646139964 ) ) ;
#10830 = DIRECTION ( 'NONE',  ( -1.000000000000000000, 0.000000000000000000, 0.000000000000000000 ) ) ;
#10831 = CARTESIAN_POINT ( 'NONE',  ( 52.25172492374522903, 53.59948385550241312, -7.007379884777225953 ) ) ;
#10832 = ADVANCED_FACE ( 'NONE', ( #3923 ), #2823, .F. ) ;
#10833 = LINE ( 'NONE', #7405, #3792 ) ;
#10834 = EDGE_CURVE ( 'NONE', #9424, #5565, #3238, .T. ) ;
#10835 = CARTESIAN_POINT ( 'NONE',  ( 45.27934281921075410, 63.29948385550240175, -6.458785618021043895 ) ) ;
#10836 = EDGE_CURVE ( 'NONE', #568, #5875, #4164, .T. ) ;
#10837 = VERTEX_POINT ( 'NONE', #8626 ) ;
#10838 = VERTEX_POINT ( 'NONE', #10758 ) ;
#10839 = ORIENTED_EDGE ( 'NONE', *, *, #10069, .F. ) ;
#10840 = LINE ( 'NONE', #7747, #4519 ) ;
#10841 = AXIS2_PLACEMENT_3D ( 'NONE', #7730, #13097, #13162 ) ;
#10842 = CARTESIAN_POINT ( 'NONE',  ( 20.00000000000000000, -20.00000000000000000, -23.00000000000000000 ) ) ;
#10843 = CARTESIAN_POINT ( 'NONE',  ( 44.91013252490150620, 54.20051614449766220, -3.727524721679154940 ) ) ;
#10844 = DIRECTION ( 'NONE',  ( -0.9768494444668812671, -0.2139279384389642935, 0.000000000000000000 ) ) ;
#10845 = CARTESIAN_POINT ( 'NONE',  ( 45.27934281921075410, 55.29948385550240175, -6.458785618021043895 ) ) ;
#10846 = ADVANCED_FACE ( 'NONE', ( #3302 ), #11498, .F. ) ;
#10847 = CARTESIAN_POINT ( 'NONE',  ( 56.66441430157296821, 54.09948385550240602, 2.141517661632100111 ) ) ;
#10848 = DIRECTION ( 'NONE',  ( -1.000000000000000000, 0.000000000000000000, -0.000000000000000000 ) ) ;
#10849 = CARTESIAN_POINT ( 'NONE',  ( 57.61547081786810764, 62.90051614449765083, -2.450534656007114176 ) ) ;
#10850 = AXIS2_PLACEMENT_3D ( 'NONE', #3961, #7081, #1740 ) ;
#10851 = VECTOR ( 'NONE', #13567, 1000.000000000000114 ) ;
#10852 = CIRCLE ( 'NONE', #4124, 1.500000000000000666 ) ;
#10853 = ORIENTED_EDGE ( 'NONE', *, *, #9559, .T. ) ;
#10854 = VERTEX_POINT ( 'NONE', #9456 ) ;
#10855 = VERTEX_POINT ( 'NONE', #3437 ) ;
#10856 = ORIENTED_EDGE ( 'NONE', *, *, #12531, .F. ) ;
#10857 = CARTESIAN_POINT ( 'NONE',  ( 1.000000000000000444, -15.10102051443364246, -8.999999999999998224 ) ) ;
#10858 = CARTESIAN_POINT ( 'NONE',  ( 62.49999999999998579, 32.50000000000001421, 15.00000000000000000 ) ) ;
#10859 =( LENGTH_UNIT ( ) NAMED_UNIT ( * ) SI_UNIT ( .MILLI., .METRE. ) );
#10860 = LINE ( 'NONE', #410, #4012 ) ;
#10861 = CARTESIAN_POINT ( 'NONE',  ( 75.00000000000001421, -7.499999999999971578, -20.00000000000000000 ) ) ;
#10862 = AXIS2_PLACEMENT_3D ( 'NONE', #251, #9473, #6254 ) ;
#10863 = CARTESIAN_POINT ( 'NONE',  ( 55.69932041026404335, 55.89948385550241028, -1.875703265242203432 ) ) ;
#10864 = CARTESIAN_POINT ( 'NONE',  ( 44.03140696652198471, 45.80051614449766362, 4.306917132069485454 ) ) ;
#10865 = CARTESIAN_POINT ( 'NONE',  ( 57.60143344285435774, 55.10051614449765367, 2.493737253992045044 ) ) ;
#10866 = DIRECTION ( 'NONE',  ( 0.000000000000000000, 0.8660254037844375974, -0.5000000000000018874 ) ) ;
#10867 = PLANE ( 'NONE',  #6690 ) ;
#10868 = CARTESIAN_POINT ( 'NONE',  ( 52.57664461997821093, 45.40051614449765793, 8.007379884777206414 ) ) ;
#10869 = EDGE_LOOP ( 'NONE', ( #6955, #4556, #1945, #3699 ) ) ;
#10870 = CARTESIAN_POINT ( 'NONE',  ( 20.00000000000000000, -14.99999999999999289, -20.00000000000000000 ) ) ;
#10871 = ORIENTED_EDGE ( 'NONE', *, *, #4617, .T. ) ;
#10872 = CARTESIAN_POINT ( 'NONE',  ( -2.915605589912154091E-15, 3.838309248099015747, 3.351853367131007566 ) ) ;
#10873 = AXIS2_PLACEMENT_3D ( 'NONE', #2636, #1659, #4793 ) ;
#10874 = DIRECTION ( 'NONE',  ( -1.000000000000000000, -0.000000000000000000, -0.000000000000000000 ) ) ;
#10875 = FACE_OUTER_BOUND ( 'NONE', #3398, .T. ) ;
#10876 = CARTESIAN_POINT ( 'NONE',  ( 20.00000000000000000, -20.00000000000000000, -27.00000000000000355 ) ) ;
#10877 = CARTESIAN_POINT ( 'NONE',  ( 47.74827507625478518, 58.59948385550238470, 7.007379884777227730 ) ) ;
#10878 = DIRECTION ( 'NONE',  ( 1.000000000000000000, 0.000000000000000000, 0.000000000000000000 ) ) ;
#10879 = CARTESIAN_POINT ( 'NONE',  ( 55.08986747509849380, 55.20051614449766220, 3.727524721679155384 ) ) ;
#10880 = FACE_OUTER_BOUND ( 'NONE', #5751, .T. ) ;
#10881 = CYLINDRICAL_SURFACE ( 'NONE', #2850, 4.800000000000000711 ) ;
#10882 = SURFACE_STYLE_USAGE ( .BOTH. , #5649 ) ;
#10883 = CARTESIAN_POINT ( 'NONE',  ( 53.50833635130540955, 47.69948385550240744, -4.867452303228209765 ) ) ;
#10884 = DIRECTION ( 'NONE',  ( 4.082155997157843695E-16, -1.000000000000000000, 0.000000000000000000 ) ) ;
#10885 = ORIENTED_EDGE ( 'NONE', *, *, #7173, .T. ) ;
#10886 = ORIENTED_EDGE ( 'NONE', *, *, #417, .T. ) ;
#10887 = UNCERTAINTY_MEASURE_WITH_UNIT (LENGTH_MEASURE( 1.000000000000000082E-05 ), #4614, 'distance_accuracy_value', 'NONE');
#10888 = ORIENTED_EDGE ( 'NONE', *, *, #1500, .F. ) ;
#10889 = LINE ( 'NONE', #10958, #6173 ) ;
#10890 = CARTESIAN_POINT ( 'NONE',  ( 2.855764796983346177, -2.970025579236428737, -0.09382832055446485575 ) ) ;
#10891 = LINE ( 'NONE', #5795, #1335 ) ;
#10892 = CARTESIAN_POINT ( 'NONE',  ( 6.207671477328661425, 5.338259717474330479, 0.7538629453361838095 ) ) ;
#10893 = CARTESIAN_POINT ( 'NONE',  ( -12.17636723815376953, -28.75991329190052781, -9.000000000000000000 ) ) ;
#10894 = EDGE_CURVE ( 'NONE', #65, #5117, #9850, .T. ) ;
#10895 = CIRCLE ( 'NONE', #10688, 2.649999999999989697 ) ;
#10896 = CARTESIAN_POINT ( 'NONE',  ( 52.29715082351538769, 50.60051614449766788, -6.992620115222796251 ) ) ;
#10897 = DIRECTION ( 'NONE',  ( 0.7969485188038759604, 0.6040472319084893016, -1.134471691914156900E-16 ) ) ;
#10898 = CARTESIAN_POINT ( 'NONE',  ( 45.90387839640214196, 50.69948385550240744, 5.676469297603166098 ) ) ;
#10899 = CARTESIAN_POINT ( 'NONE',  ( 52.62207051974839089, 64.39948385550239607, 7.992620115222770494 ) ) ;
#10900 = EDGE_CURVE ( 'NONE', #10076, #10627, #11447, .T. ) ;
#10901 = VECTOR ( 'NONE', #10252, 1000.000000000000000 ) ;
#10902 = ORIENTED_EDGE ( 'NONE', *, *, #9923, .T. ) ;
#10903 = ORIENTED_EDGE ( 'NONE', *, *, #8399, .F. ) ;
#10904 = CARTESIAN_POINT ( 'NONE',  ( 3.950233766685291137, 0.7256672287179410930, -3.499999999999844125 ) ) ;
#10905 = ADVANCED_FACE ( 'NONE', ( #5459, #9526, #9661, #7659 ), #7457, .T. ) ;
#10906 = VERTEX_POINT ( 'NONE', #7394 ) ;
#10907 = ADVANCED_FACE ( 'NONE', ( #182 ), #53, .F. ) ;
#10908 = CARTESIAN_POINT ( 'NONE',  ( 0.1217565302851044418, -2.351289329882175760, -2.927447417349501535 ) ) ;
#10909 = CIRCLE ( 'NONE', #8500, 3.500000000000000000 ) ;
#10910 = ADVANCED_FACE ( 'NONE', ( #12698 ), #6889, .T. ) ;
#10911 = AXIS2_PLACEMENT_3D ( 'NONE', #6630, #9734, #1146 ) ;
#10912 = DIRECTION ( 'NONE',  ( 9.710251638871371392E-17, 5.969973981896233748E-17, 1.000000000000000000 ) ) ;
#10913 = CARTESIAN_POINT ( 'NONE',  ( 53.54508667620424234, 56.70051614449766930, -4.840751629271188961 ) ) ;
#10914 = FACE_OUTER_BOUND ( 'NONE', #4421, .T. ) ;
#10915 = CIRCLE ( 'NONE', #1408, 15.00000000000000000 ) ;
#10916 = CARTESIAN_POINT ( 'NONE',  ( 56.79116909180255135, 55.79948385550239465, -4.963592699179005585 ) ) ;
#10917 = CARTESIAN_POINT ( 'NONE',  ( 43.33558569842703179, 55.09948385550241312, -2.141517661632099223 ) ) ;
#10918 = CARTESIAN_POINT ( 'NONE',  ( 0.000000000000000000, 0.000000000000000000, -9.999999999999998224 ) ) ;
#10919 = CIRCLE ( 'NONE', #5206, 12.49999999999999645 ) ;
#10920 = CARTESIAN_POINT ( 'NONE',  ( 45.31609314410960820, 62.30051614449766362, -6.485486291978072693 ) ) ;
#10921 = ORIENTED_EDGE ( 'NONE', *, *, #1036, .F. ) ;
#10922 = ORIENTED_EDGE ( 'NONE', *, *, #11911, .T. ) ;
#10923 = EDGE_LOOP ( 'NONE', ( #11645, #3717, #11214, #5099 ) ) ;
#10924 = ORIENTED_EDGE ( 'NONE', *, *, #99, .F. ) ;
#10925 = AXIS2_PLACEMENT_3D ( 'NONE', #5032, #13435, #10340 ) ;
#10926 = LINE ( 'NONE', #12790, #939 ) ;
#10927 = SURFACE_STYLE_FILL_AREA ( #2086 ) ;
#10928 = ADVANCED_FACE ( 'NONE', ( #6624 ), #8902, .F. ) ;
#10929 =( NAMED_UNIT ( * ) PLANE_ANGLE_UNIT ( ) SI_UNIT ( $, .RADIAN. ) );
#10930 = CYLINDRICAL_SURFACE ( 'NONE', #9321, 3.500000000000000000 ) ;
#10931 = CARTESIAN_POINT ( 'NONE',  ( -30.00000000000000000, -1.040834085586084257E-14, 0.000000000000000000 ) ) ;
#10932 = CARTESIAN_POINT ( 'NONE',  ( 56.30877334542961421, 57.99948385550241170, -0.02388180880520959434 ) ) ;
#10933 = CARTESIAN_POINT ( 'NONE',  ( 47.70284917648459810, 45.60051614449765367, 6.992620115222797139 ) ) ;
#10934 = CARTESIAN_POINT ( 'NONE',  ( 47.37792948025170858, 53.60051614449765367, 7.992620115222797139 ) ) ;
#10935 = FACE_OUTER_BOUND ( 'NONE', #11234, .T. ) ;
#10936 = DIRECTION ( 'NONE',  ( 0.000000000000000000, 0.000000000000000000, 1.000000000000000000 ) ) ;
#10937 = CARTESIAN_POINT ( 'NONE',  ( 47.37792948025170858, 45.60051614449765367, 7.992620115222797139 ) ) ;
#10938 = VERTEX_POINT ( 'NONE', #6818 ) ;
#10939 = FACE_OUTER_BOUND ( 'NONE', #11006, .T. ) ;
#10940 = EDGE_LOOP ( 'NONE', ( #7824, #7219, #3974, #1772, #332 ) ) ;
#10941 = DIRECTION ( 'NONE',  ( -0.000000000000000000, -0.000000000000000000, 1.000000000000000000 ) ) ;
#10942 = EDGE_CURVE ( 'NONE', #11193, #9043, #7923, .T. ) ;
#10943 = EDGE_CURVE ( 'NONE', #9673, #4300, #1955, .T. ) ;
#10944 = CARTESIAN_POINT ( 'NONE',  ( 2.449293598294706513E-15, -20.00000000000000000, 9.000000000000000000 ) ) ;
#10945 = CARTESIAN_POINT ( 'NONE',  ( 6.204449577088272605, 0.9975080636026212311, 5.000000000000000000 ) ) ;
#10946 = AXIS2_PLACEMENT_3D ( 'NONE', #12330, #6950, #4880 ) ;
#10947 = APPLICATION_PROTOCOL_DEFINITION ( 'draft international standard', 'automotive_design', 1998, #12286 ) ;
#10948 = CARTESIAN_POINT ( 'NONE',  ( 44.05948171654949874, 58.79948385550240886, 4.345558710429105354 ) ) ;
#10949 = CARTESIAN_POINT ( 'NONE',  ( 44.30067958973594955, 56.10051614449766078, -1.875703265242155693 ) ) ;
#10950 = LINE ( 'NONE', #3694, #8760 ) ;
#10951 = DIRECTION ( 'NONE',  ( -0.000000000000000000, -0.000000000000000000, -1.000000000000000000 ) ) ;
#10952 = CARTESIAN_POINT ( 'NONE',  ( 47.74827507625469281, 46.40051614449764372, -7.007379884777203749 ) ) ;
#10953 = CARTESIAN_POINT ( 'NONE',  ( 55.11794222512601493, 48.19948385550240744, 3.688883143319541702 ) ) ;
#10954 = FACE_OUTER_BOUND ( 'NONE', #8134, .T. ) ;
#10955 = VERTEX_POINT ( 'NONE', #3702 ) ;
#10956 = SHAPE_REPRESENTATION ( 'Mounting block', ( #430 ), #11706 ) ;
#10957 = ORIENTED_EDGE ( 'NONE', *, *, #5113, .T. ) ;
#10958 = CARTESIAN_POINT ( 'NONE',  ( -0.9999999999999976685, -20.00000000000000000, -9.000000000000001776 ) ) ;
#10959 = VECTOR ( 'NONE', #675, 1000.000000000000000 ) ;
#10960 = CARTESIAN_POINT ( 'NONE',  ( 3.355112389629172576, -2.681727112203168950, -0.2256878752776777242 ) ) ;
#10961 = CARTESIAN_POINT ( 'NONE',  ( 45.60000000000000142, 0.000000000000000000, 0.000000000000000000 ) ) ;
#10962 = CARTESIAN_POINT ( 'NONE',  ( 75.00000000000001421, -7.499999999999971578, -20.00000000000000000 ) ) ;
#10963 = DIRECTION ( 'NONE',  ( 0.000000000000000000, 0.000000000000000000, -1.000000000000000000 ) ) ;
#10964 = CARTESIAN_POINT ( 'NONE',  ( 42.63976443033212860, 56.00051614449765935, -0.02388180880514948964 ) ) ;
#10965 = CARTESIAN_POINT ( 'NONE',  ( 0.1481481481481481122, -4.797713218419819903, -1.000000000000000000 ) ) ;
#10966 = ADVANCED_FACE ( 'NONE', ( #8829 ), #5793, .F. ) ;
#10967 = CARTESIAN_POINT ( 'NONE',  ( 44.03140696652192787, 53.19948385550238612, -4.306917132069425058 ) ) ;
#10968 = CARTESIAN_POINT ( 'NONE',  ( 56.66441430157296821, 50.09948385550240602, 2.141517661632100111 ) ) ;
#10969 = CARTESIAN_POINT ( 'NONE',  ( 41.58830220609386430, 60.99948385550241170, 0.02388180880523263147 ) ) ;
#10970 = ADVANCED_FACE ( 'NONE', ( #3501, #4814, #13095 ), #2523, .F. ) ;
#10971 = ORIENTED_EDGE ( 'NONE', *, *, #8148, .T. ) ;
#10972 = ORIENTED_EDGE ( 'NONE', *, *, #8366, .T. ) ;
#10973 = DIRECTION ( 'NONE',  ( -1.000000000000000000, 0.000000000000000000, 0.000000000000000000 ) ) ;
#10974 = ORIENTED_EDGE ( 'NONE', *, *, #2293, .F. ) ;
#10975 = CARTESIAN_POINT ( 'NONE',  ( -74.99999999999997158, 32.50000000000001421, -9.999999999999998224 ) ) ;
#10976 = DIRECTION ( 'NONE',  ( 0.000000000000000000, -0.000000000000000000, 1.000000000000000000 ) ) ;
#10977 = CARTESIAN_POINT ( 'NONE',  ( 46.49166364869456913, 54.30051614449765651, -4.867452303228181343 ) ) ;
#10978 = DIRECTION ( 'NONE',  ( 0.000000000000000000, 0.000000000000000000, -1.000000000000000000 ) ) ;
#10979 = CARTESIAN_POINT ( 'NONE',  ( 49.97728705011486738, 53.49948385550240459, -8.000000000000001776 ) ) ;
#10980 = CARTESIAN_POINT ( 'NONE',  ( 52.29715082351547295, 58.39948385550238896, 6.992620115222774047 ) ) ;
#10981 = CARTESIAN_POINT ( 'NONE',  ( 6.367873360227558344, -2.886751345948133984, -5.000000000000000000 ) ) ;
#10982 = CARTESIAN_POINT ( 'NONE',  ( 52.57664461997811856, 45.59948385550240602, -8.007379884777229506 ) ) ;
#10983 = ORIENTED_EDGE ( 'NONE', *, *, #10150, .T. ) ;
#10984 = EDGE_LOOP ( 'NONE', ( #1755, #2712, #5533, #13415 ) ) ;
#10985 = ORIENTED_EDGE ( 'NONE', *, *, #12102, .F. ) ;
#10986 = VECTOR ( 'NONE', #8330, 1000.000000000000000 ) ;
#10987 = VERTEX_POINT ( 'NONE', #11096 ) ;
#10988 = DIRECTION ( 'NONE',  ( -0.000000000000000000, -0.000000000000000000, -1.000000000000000000 ) ) ;
#10989 = B_SPLINE_CURVE_WITH_KNOTS ( 'NONE', 3,
 ( #12306, #671, #10804, #4924, #13329, #3484, #11271, #6040 ),
 .UNSPECIFIED., .F., .F.,
 ( 4, 2, 2, 4 ),
 ( 0.000000000000000000, 0.002450665683189818828, 0.003675998524784728459, 0.004901331366379638524 ),
 .UNSPECIFIED. ) ;
#10990 = DIRECTION ( 'NONE',  ( 0.000000000000000000, 0.000000000000000000, 1.000000000000000000 ) ) ;
#10991 = DIRECTION ( 'NONE',  ( -0.000000000000000000, 0.000000000000000000, 1.000000000000000000 ) ) ;
#10992 = DIRECTION ( 'NONE',  ( 1.000000000000000000, 0.000000000000000000, 0.000000000000000000 ) ) ;
#10993 = CARTESIAN_POINT ( 'NONE',  ( 44.30067958973596376, 56.89948385550240317, 1.875703265242204099 ) ) ;
#10994 = CARTESIAN_POINT ( 'NONE',  ( 54.09612160359792199, 47.30051614449765651, 5.676469297603124353 ) ) ;
#10995 = CARTESIAN_POINT ( 'NONE',  ( 42.39856655714564226, 54.10051614449766078, -2.493737253992044156 ) ) ;
#10996 = AXIS2_PLACEMENT_3D ( 'NONE', #10820, #12139, #1337 ) ;
#10997 = FACE_OUTER_BOUND ( 'NONE', #4672, .T. ) ;
#10998 = LINE ( 'NONE', #2782, #482 ) ;
#10999 = EDGE_CURVE ( 'NONE', #8692, #1384, #5863, .T. ) ;
#11000 = CARTESIAN_POINT ( 'NONE',  ( 50.02271294988505446, 46.50051614449766646, -8.000000000000001776 ) ) ;
#11001 = COLOUR_RGB ( '',0.8941176470588234615, 0.8941176470588234615, 0.8941176470588234615 ) ;
#11002 = EDGE_CURVE ( 'NONE', #3041, #8508, #11220, .T. ) ;
#11003 = ORIENTED_EDGE ( 'NONE', *, *, #4329, .T. ) ;
#11004 = CYLINDRICAL_SURFACE ( 'NONE', #10805, 2.649999999999985700 ) ;
#11005 = EDGE_CURVE ( 'NONE', #12658, #7378, #11457, .T. ) ;
#11006 = EDGE_LOOP ( 'NONE', ( #7442, #11586, #12547, #9201 ) ) ;
#11007 = CIRCLE ( 'NONE', #6825, 5.000000000000000888 ) ;
#11008 = DIRECTION ( 'NONE',  ( -0.9768494444668812671, -0.2139279384389642935, 0.000000000000000000 ) ) ;
#11009 = CARTESIAN_POINT ( 'NONE',  ( 3.878096787214417862, -3.381939201670079331, -1.142309474598505181 ) ) ;
#11010 = AXIS2_PLACEMENT_3D ( 'NONE', #8891, #242, #305 ) ;
#11011 = DIRECTION ( 'NONE',  ( 0.9237280213470682178, 0.3830490080632377725, 0.000000000000000000 ) ) ;
#11012 = CARTESIAN_POINT ( 'NONE',  ( 55.96859303347804371, 56.19948385550241454, 4.306917132069425946 ) ) ;
#11013 = VECTOR ( 'NONE', #3482, 1000.000000000000000 ) ;
#11014 = CARTESIAN_POINT ( 'NONE',  ( 53.50833635130544508, 61.30051614449766362, 4.867452303228181343 ) ) ;
#11015 = DIRECTION ( 'NONE',  ( -1.000000000000000000, 0.000000000000000000, 0.000000000000000000 ) ) ;
#11016 = CARTESIAN_POINT ( 'NONE',  ( 0.000000000000000000, 0.000000000000000000, 8.999999999999998224 ) ) ;
#11017 = CARTESIAN_POINT ( 'NONE',  ( 56.65037692655921120, 47.10051614449766078, 2.184720259617097593 ) ) ;
#11018 = CARTESIAN_POINT ( 'NONE',  ( 44.88205777487398507, 49.19948385550240744, -3.688883143319540814 ) ) ;
#11019 = AXIS2_PLACEMENT_3D ( 'NONE', #4634, #10716, #7817 ) ;
#11020 = DIRECTION ( 'NONE',  ( -0.000000000000000000, -0.000000000000000000, 1.000000000000000000 ) ) ;
#11021 = VERTEX_POINT ( 'NONE', #7861 ) ;
#11022 = PRODUCT_DEFINITION_CONTEXT ( 'detailed design', #11126, 'design' ) ;
#11023 = EDGE_LOOP ( 'NONE', ( #1305, #670, #12389, #13243 ) ) ;
#11024 = FACE_OUTER_BOUND ( 'NONE', #11423, .T. ) ;
#11025 = CARTESIAN_POINT ( 'NONE',  ( 0.5469614295415388128, -4.303013824935362663, -3.535263753543555598 ) ) ;
#11026 = LINE ( 'NONE', #4750, #1555 ) ;
#11027 = ADVANCED_FACE ( 'NONE', ( #11932, #11024 ), #1543, .T. ) ;
#11028 = CIRCLE ( 'NONE', #2877, 15.00000000000000000 ) ;
#11029 = CARTESIAN_POINT ( 'NONE',  ( 7.500000000000107470, -32.99038105676652322, 9.000000000000000000 ) ) ;
#11030 = DIRECTION ( 'NONE',  ( -1.000000000000000000, 0.000000000000000000, 0.000000000000000000 ) ) ;
#11031 = CARTESIAN_POINT ( 'NONE',  ( 54.13287192849671214, 62.70051614449766220, -5.649768623646139964 ) ) ;
#11032 = CARTESIAN_POINT ( 'NONE',  ( 6.541333988313477121, -2.987057409892287740, -5.112749828287758369 ) ) ;
#11033 = LINE ( 'NONE', #12352, #12248 ) ;
#11034 = CARTESIAN_POINT ( 'NONE',  ( 44.03140696652192787, 55.19948385550238612, -4.306917132069425058 ) ) ;
#11035 = CARTESIAN_POINT ( 'NONE',  ( 56.65037692655918988, 49.89948385550240317, -2.184720259617163762 ) ) ;
#11036 = SHAPE_REPRESENTATION ( 'motor', ( #430 ), #10821 ) ;
#11037 = CARTESIAN_POINT ( 'NONE',  ( 56.79116909180255135, 61.79948385550240175, -4.963592699179005585 ) ) ;
#11038 =( GEOMETRIC_REPRESENTATION_CONTEXT ( 3 ) GLOBAL_UNCERTAINTY_ASSIGNED_CONTEXT ( ( #4539 ) ) GLOBAL_UNIT_ASSIGNED_CONTEXT ( ( #10304, #4017, #601 ) ) REPRESENTATION_CONTEXT ( 'NONE', 'WORKASPACE' ) );
#11039 = ORIENTED_EDGE ( 'NONE', *, *, #2899, .T. ) ;
#11040 = EDGE_LOOP ( 'NONE', ( #10644, #8623, #8202, #8183, #12233 ) ) ;
#11041 = CARTESIAN_POINT ( 'NONE',  ( 3.972073812946708582, -0.6951863858492246528, -3.565770933504603057 ) ) ;
#11042 = VERTEX_POINT ( 'NONE', #4747 ) ;
#11043 = CARTESIAN_POINT ( 'NONE',  ( 0.1381419387119174058, -1.355287006778759018, 3.500000000000000888 ) ) ;
#11044 = EDGE_CURVE ( 'NONE', #8372, #3318, #4384, .T. ) ;
#11045 = CARTESIAN_POINT ( 'NONE',  ( 4.175813232069146785, 2.061359961916365613, -3.570380186727397653 ) ) ;
#11046 = CARTESIAN_POINT ( 'NONE',  ( 53.50833635130544508, 53.30051614449767072, 4.867452303228181343 ) ) ;
#11047 = PRODUCT ( 'hex flange bolt small_iso_ISO 4162 - M8 x 45 x 22-N', 'hex flange bolt small_iso_ISO 4162 - M8 x 45 x 22-N', '', ( #766 ) ) ;
#11048 = CYLINDRICAL_SURFACE ( 'NONE', #10801, 1.999999999999998224 ) ;
#11049 = CARTESIAN_POINT ( 'NONE',  ( 56.79116909180255135, 53.79948385550241596, -4.963592699179005585 ) ) ;
#11050 = CARTESIAN_POINT ( 'NONE',  ( 52.25172492374522903, 59.59948385550240602, -7.007379884777225953 ) ) ;
#11051 = CARTESIAN_POINT ( 'NONE',  ( -4.154094228333456762, 2.398367420968013253, -3.721909803043220055 ) ) ;
#11052 = CARTESIAN_POINT ( 'NONE',  ( 43.20883090819742023, 62.20051614449766220, -4.963592699178938972 ) ) ;
#11053 = ORIENTED_EDGE ( 'NONE', *, *, #11473, .F. ) ;
#11054 = ITEM_DEFINED_TRANSFORMATION ( 'NONE', 'NONE', #1077,  #430 ) ;
#11055 = CIRCLE ( 'NONE', #7757, 15.00000000000000000 ) ;
#11056 = VERTEX_POINT ( 'NONE', #10054 ) ;
#11057 = ORIENTED_EDGE ( 'NONE', *, *, #2665, .T. ) ;
#11058 = VERTEX_POINT ( 'NONE', #8762 ) ;
#11059 = CYLINDRICAL_SURFACE ( 'NONE', #2603, 15.00000000000000000 ) ;
#11060 = CARTESIAN_POINT ( 'NONE',  ( 2.000000000000005329, -3.464101615137751722, 0.000000000000000000 ) ) ;
#11061 = CARTESIAN_POINT ( 'NONE',  ( 49.99999999999997158, 45.00000000000001421, -7.000000000000000888 ) ) ;
#11062 = CARTESIAN_POINT ( 'NONE',  ( 48.07319477248768180, 56.59948385550239891, 6.007379884777225953 ) ) ;
#11063 = CARTESIAN_POINT ( 'NONE',  ( 43.34962307344078880, 48.10051614449766078, -2.184720259617096705 ) ) ;
#11064 = CARTESIAN_POINT ( 'NONE',  ( 43.18075615816994173, 49.80051614449765651, 4.924951120819380357 ) ) ;
#11065 = AXIS2_PLACEMENT_3D ( 'NONE', #8260, #5085, #12463 ) ;
#11066 = AXIS2_PLACEMENT_3D ( 'NONE', #1353, #8705, #4351 ) ;
#11067 = CYLINDRICAL_SURFACE ( 'NONE', #6480, 5.000000000000000000 ) ;
#11068 = AXIS2_PLACEMENT_3D ( 'NONE', #110, #3291, #10751 ) ;
#11069 = EDGE_CURVE ( 'NONE', #4695, #8677, #13027, .T. ) ;
#11070 = CARTESIAN_POINT ( 'NONE',  ( 49.97728705011495265, 63.50051614449765935, 7.000000000000000888 ) ) ;
#11071 = ORIENTED_EDGE ( 'NONE', *, *, #12483, .T. ) ;
#11072 = CARTESIAN_POINT ( 'NONE',  ( -1.312671235360383548, -3.860931062424228788, -0.05923475698271369466 ) ) ;
#11073 = ADVANCED_FACE ( 'NONE', ( #7996 ), #7797, .F. ) ;
#11074 = EDGE_LOOP ( 'NONE', ( #6214, #5419, #11618, #11861 ) ) ;
#11075 = AXIS2_PLACEMENT_3D ( 'NONE', #7663, #4475, #8698 ) ;
#11076 = VECTOR ( 'NONE', #10045, 1000.000000000000114 ) ;
#11077 = EDGE_CURVE ( 'NONE', #6557, #7826, #10889, .T. ) ;
#11078 = CARTESIAN_POINT ( 'NONE',  ( 0.3126073911696427010, 4.041451884327382338, -6.521455134176256610E-17 ) ) ;
#11079 = DIRECTION ( 'NONE',  ( 1.000000000000000000, 0.000000000000000000, 0.000000000000000000 ) ) ;
#11080 = EDGE_CURVE ( 'NONE', #7826, #13382, #5655, .T. ) ;
#11081 = EDGE_CURVE ( 'NONE', #7907, #11125, #189, .T. ) ;
#11082 =( LENGTH_UNIT ( ) NAMED_UNIT ( * ) SI_UNIT ( .MILLI., .METRE. ) );
#11083 = CARTESIAN_POINT ( 'NONE',  ( 45.86712807150323812, 55.29948385550240175, -5.649768623646098220 ) ) ;
#11084 = CARTESIAN_POINT ( 'NONE',  ( 47.70284917648453415, 51.39948385550240317, -6.992620115222774047 ) ) ;
#11085 = CARTESIAN_POINT ( 'NONE',  ( 44.88205777487401349, 55.80051614449766362, 3.688883143319584779 ) ) ;
#11086 = DIRECTION ( 'NONE',  ( -1.000000000000000000, -0.000000000000000000, -0.000000000000000000 ) ) ;
#11087 = CARTESIAN_POINT ( 'NONE',  ( -74.99999999999998579, 7.499999999999975131, 10.00000000000000000 ) ) ;
#11088 = EDGE_CURVE ( 'NONE', #898, #12709, #3925, .T. ) ;
#11089 = CARTESIAN_POINT ( 'NONE',  ( 50.02271294988506156, 62.50051614449767357, -6.000000000000000888 ) ) ;
#11090 = CARTESIAN_POINT ( 'NONE',  ( 53.50833635130540955, 45.69948385550240033, -4.867452303228209765 ) ) ;
#11091 = CARTESIAN_POINT ( 'NONE',  ( 2.000000000000000000, 1.773042676681340524, -2.059984127722458425E-15 ) ) ;
#11092 = ORIENTED_EDGE ( 'NONE', *, *, #12945, .F. ) ;
#11093 = CIRCLE ( 'NONE', #59, 2.649999999999985700 ) ;
#11094 = ORIENTED_EDGE ( 'NONE', *, *, #10836, .T. ) ;
#11095 = ORIENTED_EDGE ( 'NONE', *, *, #6753, .F. ) ;
#11096 = CARTESIAN_POINT ( 'NONE',  ( 75.00000000000001421, -39.99999999999998579, -20.00000000000000000 ) ) ;
#11097 = VECTOR ( 'NONE', #11424, 1000.000000000000000 ) ;
#11098 = DIRECTION ( 'NONE',  ( 0.000000000000000000, 0.000000000000000000, 1.000000000000000000 ) ) ;
#11099 = DIRECTION ( 'NONE',  ( -1.000000000000000000, 0.000000000000000000, 0.000000000000000000 ) ) ;
#11100 = CARTESIAN_POINT ( 'NONE',  ( 6.506891779418573662, 2.833891091414751706, 5.091556646552823473 ) ) ;
#11101 = CARTESIAN_POINT ( 'NONE',  ( 25.00000000000000711, -20.00000000000000000, -23.00000000000000000 ) ) ;
#11102 = VECTOR ( 'NONE', #11960, 1000.000000000000000 ) ;
#11103 = CARTESIAN_POINT ( 'NONE',  ( 55.94051828345053679, 63.20051614449765509, 4.345558710429044069 ) ) ;
#11104 = CYLINDRICAL_SURFACE ( 'NONE', #10595, 1.500000000000001332 ) ;
#11105 = CARTESIAN_POINT ( 'NONE',  ( 4.071447262713888016, 4.041451884327382338, 0.000000000000000000 ) ) ;
#11106 = CARTESIAN_POINT ( 'NONE',  ( 55.96859303347804371, 58.19948385550241454, 4.306917132069425946 ) ) ;
#11107 =( NAMED_UNIT ( * ) PLANE_ANGLE_UNIT ( ) SI_UNIT ( $, .RADIAN. ) );
#11108 = CARTESIAN_POINT ( 'NONE',  ( 47.70284917648453415, 51.39948385550238896, -6.992620115222774047 ) ) ;
#11109 = ORIENTED_EDGE ( 'NONE', *, *, #11911, .F. ) ;
#11110 = ORIENTED_EDGE ( 'NONE', *, *, #12031, .F. ) ;
#11111 = CARTESIAN_POINT ( 'NONE',  ( 0.000000000000000000, 0.000000000000000000, -1.000000000000000000 ) ) ;
#11112 = VERTEX_POINT ( 'NONE', #7097 ) ;
#11113 = CARTESIAN_POINT ( 'NONE',  ( 6.244297270354684848, -1.798312406574552930E-11, -5.105276777067894400 ) ) ;
#11114 = ADVANCED_FACE ( 'NONE', ( #10271 ), #7243, .T. ) ;
#11115 = CARTESIAN_POINT ( 'NONE',  ( 6.196878017913834746, -5.292377467571577121, -0.8333333333333331483 ) ) ;
#11116 = CARTESIAN_POINT ( 'NONE',  ( 50.02271294988506156, 62.50051614449767357, -6.000000000000000888 ) ) ;
#11117 = CARTESIAN_POINT ( 'NONE',  ( 50.00000000000000000, 15.00000000000000000, 4.000000000000003553 ) ) ;
#11118 = CARTESIAN_POINT ( 'NONE',  ( 57.61547081786812896, 62.09948385550240602, 2.450534656007040901 ) ) ;
#11119 = CARTESIAN_POINT ( 'NONE',  ( 56.66441430157296821, 60.09948385550240602, 2.141517661632100111 ) ) ;
#11120 = DIRECTION ( 'NONE',  ( 0.000000000000000000, 0.000000000000000000, 1.000000000000000000 ) ) ;
#11121 = AXIS2_PLACEMENT_3D ( 'NONE', #5157, #9363, #11149 ) ;
#11122 = CARTESIAN_POINT ( 'NONE',  ( 52.62207051974829852, 62.60051614449765367, -7.992620115222797139 ) ) ;
#11123 = ORIENTED_EDGE ( 'NONE', *, *, #5211, .T. ) ;
#11124 = VECTOR ( 'NONE', #2870, 1000.000000000000000 ) ;
#11125 = VERTEX_POINT ( 'NONE', #7023 ) ;
#11126 = APPLICATION_CONTEXT ( 'automotive_design' ) ;
#11127 = ORIENTED_EDGE ( 'NONE', *, *, #9895, .F. ) ;
#11128 = EDGE_LOOP ( 'NONE', ( #5755, #4203, #7571, #5924 ) ) ;
#11129 = AXIS2_PLACEMENT_3D ( 'NONE', #7194, #6162, #11546 ) ;
#11130 = CARTESIAN_POINT ( 'NONE',  ( 13.67449106481161003, -13.83491329190030861, -9.000000000000000000 ) ) ;
#11131 = CIRCLE ( 'NONE', #8506, 5.000000000000000000 ) ;
#11132 = DIRECTION ( 'NONE',  ( 1.000000000000000000, 0.000000000000000000, 0.000000000000000000 ) ) ;
#11133 = CARTESIAN_POINT ( 'NONE',  ( 0.6666666666666658525, -4.233901974057276085, -3.300726591567086476 ) ) ;
#11134 = CARTESIAN_POINT ( 'NONE',  ( 0.1973348417602470706, -1.936114729415141733, 4.999999999999999112 ) ) ;
#11135 = CARTESIAN_POINT ( 'NONE',  ( 48.07319477248768180, 62.59948385550238470, 6.007379884777225953 ) ) ;
#11136 = CARTESIAN_POINT ( 'NONE',  ( 52.29715082351539479, 50.60051614449766078, -6.992620115222796251 ) ) ;
#11137 = AXIS2_PLACEMENT_3D ( 'NONE', #1909, #7386, #9248 ) ;
#11138 = CARTESIAN_POINT ( 'NONE',  ( 54.68390685589039890, 51.30051614449765651, 6.485486291978072693 ) ) ;
#11139 = FACE_OUTER_BOUND ( 'NONE', #8990, .T. ) ;
#11140 = DIRECTION ( 'NONE',  ( 0.000000000000000000, 1.000000000000000000, 0.000000000000000000 ) ) ;
#11141 = ADVANCED_FACE ( 'NONE', ( #1683 ), #635, .F. ) ;
#11142 = CARTESIAN_POINT ( 'NONE',  ( 45.86712807150329496, 61.70051614449766220, 5.649768623646139964 ) ) ;
#11143 = CIRCLE ( 'NONE', #8718, 15.00000000000000000 ) ;
#11145 = ORIENTED_EDGE ( 'NONE', *, *, #8814, .F. ) ;
#11144 = VERTEX_POINT ( 'NONE', #5174 ) ;
#11146 = DIRECTION ( 'NONE',  ( 0.000000000000000000, 0.000000000000000000, 1.000000000000000000 ) ) ;
#11147 = EDGE_CURVE ( 'NONE', #5892, #9150, #11007, .T. ) ;
#11148 = ORIENTED_EDGE ( 'NONE', *, *, #9825, .F. ) ;
#11149 = DIRECTION ( 'NONE',  ( 1.000000000000000000, 0.000000000000000000, 0.000000000000000000 ) ) ;
#11150 = FACE_OUTER_BOUND ( 'NONE', #11632, .T. ) ;
#11151 =( NAMED_UNIT ( * ) SI_UNIT ( $, .STERADIAN. ) SOLID_ANGLE_UNIT ( ) );
#11152 = CARTESIAN_POINT ( 'NONE',  ( 54.13287192849676188, 54.29948385550240886, 5.649768623646098220 ) ) ;
#11153 = CARTESIAN_POINT ( 'NONE',  ( 57.36023556966787851, 57.99948385550240459, -0.02388180880522424582 ) ) ;
#11154 = LINE ( 'NONE', #3965, #11076 ) ;
#11155 = EDGE_CURVE ( 'NONE', #2434, #11144, #6604, .T. ) ;
#11156 = CARTESIAN_POINT ( 'NONE',  ( 2.000000000000000000, -6.429618962271402616, -1.000000000000000000 ) ) ;
#11157 = CARTESIAN_POINT ( 'NONE',  ( 30.00000000000000000, -4.999999999999989342, 6.123233995736775157E-16 ) ) ;
#11158 = CARTESIAN_POINT ( 'NONE',  ( 56.66441430157294690, 44.90051614449765793, -2.141517661632166281 ) ) ;
#11159 = CARTESIAN_POINT ( 'NONE',  ( 46.45491332379572924, 53.29948385550240886, -4.840751629271157874 ) ) ;
#11160 = CARTESIAN_POINT ( 'NONE',  ( -6.165086708099442703, -33.67449106481171839, -9.000000000000000000 ) ) ;
#11161 = ADVANCED_FACE ( 'NONE', ( #5031 ), #9906, .T. ) ;
#11162 = ORIENTED_EDGE ( 'NONE', *, *, #1426, .F. ) ;
#11163 = EDGE_CURVE ( 'NONE', #4186, #4189, #3978, .T. ) ;
#11164 = ORIENTED_EDGE ( 'NONE', *, *, #590, .F. ) ;
#11165 = VERTEX_POINT ( 'NONE', #10409 ) ;
#11166 = DIRECTION ( 'NONE',  ( 0.000000000000000000, -1.000000000000000000, 0.000000000000000000 ) ) ;
#11167 = CARTESIAN_POINT ( 'NONE',  ( 4.175648173966055587, -2.207990556236547608, -3.469390959564065291 ) ) ;
#11168 = CARTESIAN_POINT ( 'NONE',  ( 1.411581201560190495E-15, 4.862606272033091592, -3.745885042887436622 ) ) ;
#11169 = DIRECTION ( 'NONE',  ( -0.000000000000000000, -0.000000000000000000, 1.000000000000000000 ) ) ;
#11170 = CARTESIAN_POINT ( 'NONE',  ( 4.132952817037866211, -2.031684012687259511, 3.518979934899751250 ) ) ;
#11171 = CARTESIAN_POINT ( 'NONE',  ( 49.97728705011495265, 61.50051614449765935, 7.000000000000000888 ) ) ;
#11172 = CARTESIAN_POINT ( 'NONE',  ( 3.309651814758565180, -5.455921364805393026, -1.000000000000000000 ) ) ;
#11173 = CARTESIAN_POINT ( 'NONE',  ( 43.69122665457040000, 48.00051614449766646, -0.02388180880515696977 ) ) ;
#11174 = DIRECTION ( 'NONE',  ( 1.000000000000000000, -0.000000000000000000, 0.000000000000000000 ) ) ;
#11175 = CARTESIAN_POINT ( 'NONE',  ( 52.29715082351547295, 60.39948385550239607, 6.992620115222774047 ) ) ;
#11176 = CARTESIAN_POINT ( 'NONE',  ( 54.13287192849676188, 46.29948385550240886, 5.649768623646098220 ) ) ;
#11177 = VECTOR ( 'NONE', #13425, 1000.000000000000000 ) ;
#11178 = CARTESIAN_POINT ( 'NONE',  ( 44.05948171654949874, 46.79948385550238754, 4.345558710429105354 ) ) ;
#11179 = AXIS2_PLACEMENT_3D ( 'NONE', #9140, #3880, #7139 ) ;
#11180 = EDGE_LOOP ( 'NONE', ( #4714, #2908, #118, #2755, #7486, #3890, #4286, #10885 ) ) ;
#11181 = EDGE_LOOP ( 'NONE', ( #5351, #12549, #4642 ) ) ;
#11182 = LINE ( 'NONE', #1701, #9014 ) ;
#11183 = ORIENTED_EDGE ( 'NONE', *, *, #11044, .F. ) ;
#11184 = DIRECTION ( 'NONE',  ( 0.000000000000000000, 0.000000000000000000, -1.000000000000000000 ) ) ;
#11185 = CARTESIAN_POINT ( 'NONE',  ( 6.527192678185835817, -2.941622124011024297, -5.095038975456044561 ) ) ;
#11186 = CARTESIAN_POINT ( 'NONE',  ( 51.97223112728249816, 62.60051614449765367, -5.992620115222793586 ) ) ;
#11187 = DIRECTION ( 'NONE',  ( -0.000000000000000000, -0.000000000000000000, -1.000000000000000000 ) ) ;
#11188 = CARTESIAN_POINT ( 'NONE',  ( 52.62207051974839089, 56.39948385550241028, 7.992620115222770494 ) ) ;
#11189 = CARTESIAN_POINT ( 'NONE',  ( 54.09612160359786515, 63.69948385550240744, -5.676469297603166098 ) ) ;
#11190 = DIRECTION ( 'NONE',  ( 0.04542589977017006536, -0.9989677110047503472, 0.000000000000000000 ) ) ;
#11191 = EDGE_CURVE ( 'NONE', #4030, #6599, #4174, .T. ) ;
#11192 = CARTESIAN_POINT ( 'NONE',  ( 45.31609314410967926, 48.69948385550241454, 6.485486291978119766 ) ) ;
#11193 = VERTEX_POINT ( 'NONE', #4960 ) ;
#11194 = CONTEXT_DEPENDENT_SHAPE_REPRESENTATION ( #2382, #2344 ) ;
#11195 = ORIENTED_EDGE ( 'NONE', *, *, #11005, .T. ) ;
#11196 = ORIENTED_EDGE ( 'NONE', *, *, #10558, .T. ) ;
#11197 = ORIENTED_EDGE ( 'NONE', *, *, #5699, .T. ) ;
#11198 = DIRECTION ( 'NONE',  ( 0.000000000000000000, 0.000000000000000000, -1.000000000000000000 ) ) ;
#11199 = CARTESIAN_POINT ( 'NONE',  ( 12.99038105676665289, -27.49999999999988276, -9.000000000000000000 ) ) ;
#11200 = PRESENTATION_STYLE_ASSIGNMENT (( #1721 ) ) ;
#11201 = CARTESIAN_POINT ( 'NONE',  ( -62.49999999999997158, 32.50000000000001421, -15.00000000000000000 ) ) ;
#11202 = DIRECTION ( 'NONE',  ( 0.000000000000000000, 0.000000000000000000, -1.000000000000000000 ) ) ;
#11203 = LINE ( 'NONE', #478, #10071 ) ;
#11204 = CARTESIAN_POINT ( 'NONE',  ( 44.30067958973596376, 60.89948385550241028, 1.875703265242204099 ) ) ;
#11205 = CARTESIAN_POINT ( 'NONE',  ( 54.13287192849671214, 50.70051614449766220, -5.649768623646139964 ) ) ;
#11206 = CARTESIAN_POINT ( 'NONE',  ( 54.68390685589039890, 57.30051614449767072, 6.485486291978072693 ) ) ;
#11207 = CARTESIAN_POINT ( 'NONE',  ( 1.677125235563514178E-16, 0.3423821193476823121, 3.500000000000000444 ) ) ;
#11208 = DIRECTION ( 'NONE',  ( 0.000000000000000000, -0.000000000000000000, 1.000000000000000000 ) ) ;
#11209 = CARTESIAN_POINT ( 'NONE',  ( 49.97728705011495265, 49.50051614449766646, 8.000000000000001776 ) ) ;
#11210 = PRESENTATION_LAYER_ASSIGNMENT (  '', '', ( #2828 ) ) ;
#11212 = ORIENTED_EDGE ( 'NONE', *, *, #9986, .F. ) ;
#11211 = ORIENTED_EDGE ( 'NONE', *, *, #4180, .F. ) ;
#11213 = CARTESIAN_POINT ( 'NONE',  ( 1.312671235360372224, 3.860931062424219462, -0.05923475698270440348 ) ) ;
#11214 = ORIENTED_EDGE ( 'NONE', *, *, #505, .T. ) ;
#11215 = ORIENTED_EDGE ( 'NONE', *, *, #2081, .T. ) ;
#11216 = LINE ( 'NONE', #13350, #10901 ) ;
#11217 = FACE_OUTER_BOUND ( 'NONE', #3873, .T. ) ;
#11218 = PRODUCT_CONTEXT ( 'NONE', #12976, 'mechanical' ) ;
#11219 = CARTESIAN_POINT ( 'NONE',  ( 44.03140696652192787, 65.19948385550240744, -4.306917132069425058 ) ) ;
#11220 = CIRCLE ( 'NONE', #12552, 12.50000000000000000 ) ;
#11221 = EDGE_CURVE ( 'NONE', #5652, #3771, #1760, .T. ) ;
#11222 = CARTESIAN_POINT ( 'NONE',  ( 43.33558569842703179, 61.09948385550240602, -2.141517661632099223 ) ) ;
#11223 = MECHANICAL_DESIGN_GEOMETRIC_PRESENTATION_REPRESENTATION (  '', ( #10353 ), #13202 ) ;
#11224 = DIRECTION ( 'NONE',  ( 0.000000000000000000, 0.000000000000000000, 1.000000000000000000 ) ) ;
#11225 = EDGE_CURVE ( 'NONE', #13443, #10405, #12337, .T. ) ;
#11226 = DIRECTION ( 'NONE',  ( -0.000000000000000000, -0.000000000000000000, -1.000000000000000000 ) ) ;
#11227 = LINE ( 'NONE', #4951, #5580 ) ;
#11228 = CARTESIAN_POINT ( 'NONE',  ( 44.30067958973594955, 64.10051614449766078, -1.875703265242155693 ) ) ;
#11229 = CARTESIAN_POINT ( 'NONE',  ( 46.45491332379572924, 51.29948385550240175, -4.840751629271157874 ) ) ;
#11230 = DIRECTION ( 'NONE',  ( 1.000000000000000000, 0.000000000000000000, 0.000000000000000000 ) ) ;
#11231 = ORIENTED_EDGE ( 'NONE', *, *, #5188, .T. ) ;
#11232 = CIRCLE ( 'NONE', #10360, 3.500000000000000000 ) ;
#11233 = ORIENTED_EDGE ( 'NONE', *, *, #9017, .F. ) ;
#11234 = EDGE_LOOP ( 'NONE', ( #6768, #12659, #8454, #2537 ) ) ;
#11235 = DIRECTION ( 'NONE',  ( 0.000000000000000000, 0.000000000000000000, -1.000000000000000000 ) ) ;
#11236 = AXIS2_PLACEMENT_3D ( 'NONE', #8553, #3292, #9518 ) ;
#11237 = CARTESIAN_POINT ( 'NONE',  ( 2.482347295856823136E-15, -20.00000000000000000, -8.999999999999996447 ) ) ;
#11238 = CARTESIAN_POINT ( 'NONE',  ( 2.449293598294706513E-15, -20.00000000000000000, 9.000000000000000000 ) ) ;
#11239 = CARTESIAN_POINT ( 'NONE',  ( 54.09612160359786515, 45.69948385550240744, -5.676469297603166098 ) ) ;
#11240 = DIRECTION ( 'NONE',  ( 0.000000000000000000, 0.000000000000000000, 1.000000000000000000 ) ) ;
#11241 =( GEOMETRIC_REPRESENTATION_CONTEXT ( 3 ) GLOBAL_UNCERTAINTY_ASSIGNED_CONTEXT ( ( #9919 ) ) GLOBAL_UNIT_ASSIGNED_CONTEXT ( ( #10825, #318, #4474 ) ) REPRESENTATION_CONTEXT ( 'NONE', 'WORKASPACE' ) );
#11242 = CARTESIAN_POINT ( 'NONE',  ( 0.000000000000000000, 0.000000000000000000, 10.00000000000000000 ) ) ;
#11243 = CARTESIAN_POINT ( 'NONE',  ( 48.02776887271745210, 63.39948385550238896, -5.992620115222778487 ) ) ;
#11244 = CARTESIAN_POINT ( 'NONE',  ( -13.49999999999999467, -20.00000000000005329, -9.000000000000000000 ) ) ;
#11245 = CARTESIAN_POINT ( 'NONE',  ( 47.74827507625478518, 58.59948385550238470, 7.007379884777227730 ) ) ;
#11246 = CARTESIAN_POINT ( 'NONE',  ( 52.29715082351547295, 52.39948385550241738, 6.992620115222774047 ) ) ;
#11247 = EDGE_CURVE ( 'NONE', #4571, #10373, #10125, .T. ) ;
#11248 = EDGE_LOOP ( 'NONE', ( #2835, #9046, #5112, #8359 ) ) ;
#11249 = CARTESIAN_POINT ( 'NONE',  ( 52.29715082351547295, 50.39948385550240317, 6.992620115222774047 ) ) ;
#11250 = ORIENTED_EDGE ( 'NONE', *, *, #5470, .F. ) ;
#11251 = VERTEX_POINT ( 'NONE', #9102 ) ;
#11252 = PRODUCT_DEFINITION_FORMATION_WITH_SPECIFIED_SOURCE ( 'ANY', '', #7778, .NOT_KNOWN. ) ;
#11253 = DIRECTION ( 'NONE',  ( -0.000000000000000000, 0.000000000000000000, -1.000000000000000000 ) ) ;
#11254 = CIRCLE ( 'NONE', #10146, 2.649999999999988809 ) ;
#11255 = VERTEX_POINT ( 'NONE', #6414 ) ;
#11256 = CARTESIAN_POINT ( 'NONE',  ( 4.175075985190095373, 2.060370777630105898, 3.568666869285574972 ) ) ;
#11257 = CARTESIAN_POINT ( 'NONE',  ( 22.14999999999999858, -20.00000000000000000, -23.00000000000000000 ) ) ;
#11258 = DIRECTION ( 'NONE',  ( 1.000000000000000000, 0.000000000000000000, 0.000000000000000000 ) ) ;
#11259 = EDGE_CURVE ( 'NONE', #8692, #3281, #12121, .T. ) ;
#11260 = CARTESIAN_POINT ( 'NONE',  ( 43.69122665457040000, 58.00051614449765935, -0.02388180880515696977 ) ) ;
#11261 = ADVANCED_FACE ( 'NONE', ( #1120, #32 ), #9709, .F. ) ;
#11262 = CARTESIAN_POINT ( 'NONE',  ( 6.367873360227556567, 2.886751345948125991, 4.999999999999999112 ) ) ;
#11263 = CARTESIAN_POINT ( 'NONE',  ( 41.58830220609386430, 60.99948385550241170, 0.02388180880523263147 ) ) ;
#11264 = AXIS2_PLACEMENT_3D ( 'NONE', #11172, #6005, #1691 ) ;
#11265 = DIRECTION ( 'NONE',  ( -9.710251638871371392E-17, -5.969973981896233748E-17, -1.000000000000000000 ) ) ;
#11266 = DIRECTION ( 'NONE',  ( 1.000000000000000000, -9.251858538542972814E-17, 0.000000000000000000 ) ) ;
#11267 = CARTESIAN_POINT ( 'NONE',  ( 42.39856655714566358, 52.89948385550241028, 2.493737253992119207 ) ) ;
#11268 = ORIENTED_EDGE ( 'NONE', *, *, #1200, .T. ) ;
#11269 = ORIENTED_EDGE ( 'NONE', *, *, #3924, .T. ) ;
#11270 = VERTEX_POINT ( 'NONE', #12808 ) ;
#11271 = CARTESIAN_POINT ( 'NONE',  ( -3.861362476283256129, -2.629030857716004199, -3.671615880910374941 ) ) ;
#11272 = CYLINDRICAL_SURFACE ( 'NONE', #1254, 0.7499999999999997780 ) ;
#11273 = AXIS2_PLACEMENT_3D ( 'NONE', #6043, #1723, #2776 ) ;
#11274 = CARTESIAN_POINT ( 'NONE',  ( 4.158921614371307030, 1.986121848748763741, -3.559936047944503912 ) ) ;
#11275 = CARTESIAN_POINT ( 'NONE',  ( 3.951447005078453589, -3.704664227300103807, 0.5833333333333329263 ) ) ;
#11276 = EDGE_CURVE ( 'NONE', #5998, #8131, #6420, .T. ) ;
#11277 = DIRECTION ( 'NONE',  ( 0.000000000000000000, 1.000000000000000000, 0.000000000000000000 ) ) ;
#11278 = CARTESIAN_POINT ( 'NONE',  ( 56.30877334542961421, 45.00051614449765225, 0.02388180880515774693 ) ) ;
#11279 = CARTESIAN_POINT ( 'NONE',  ( 42.63976443033212149, 54.00051614449765935, -0.02388180880514948964 ) ) ;
#11280 = CARTESIAN_POINT ( 'NONE',  ( 49.97728705011495265, 59.50051614449765935, 8.000000000000001776 ) ) ;
#11281 = DIRECTION ( 'NONE',  ( 0.000000000000000000, 0.000000000000000000, 1.000000000000000000 ) ) ;
#11282 = CARTESIAN_POINT ( 'NONE',  ( 43.18075615816994173, 47.80051614449764941, 4.924951120819380357 ) ) ;
#11284 = EDGE_LOOP ( 'NONE', ( #6991, #8253 ) ) ;
#11283 = ORIENTED_EDGE ( 'NONE', *, *, #12763, .F. ) ;
#11285 = EDGE_CURVE ( 'NONE', #10489, #11319, #2179, .T. ) ;
#11286 = DIRECTION ( 'NONE',  ( 1.000000000000000000, 0.000000000000000000, 0.000000000000000000 ) ) ;
#11287 = ORIENTED_EDGE ( 'NONE', *, *, #6862, .F. ) ;
#11288 = ORIENTED_EDGE ( 'NONE', *, *, #12963, .F. ) ;
#11289 = CARTESIAN_POINT ( 'NONE',  ( 75.00000000000001421, 7.500000000000027534, 10.00000000000000000 ) ) ;
#11290 = DIRECTION ( 'NONE',  ( 0.000000000000000000, 0.000000000000000000, 1.000000000000000000 ) ) ;
#11291 = AXIS2_PLACEMENT_3D ( 'NONE', #7298, #11507, #975 ) ;
#11292 = APPLICATION_PROTOCOL_DEFINITION ( 'draft international standard', 'automotive_design', 1998, #3544 ) ;
#11293 = CARTESIAN_POINT ( 'NONE',  ( 47.70284917648453415, 63.39948385550240317, -6.992620115222774047 ) ) ;
#11294=STYLED_ITEM('',(#13712),#5623);
#11295 = CARTESIAN_POINT ( 'NONE',  ( 56.65037692655918988, 55.89948385550240317, -2.184720259617163762 ) ) ;
#11296 = PLANE ( 'NONE',  #1900 ) ;
#11297 = CARTESIAN_POINT ( 'NONE',  ( 6.244297270354683960, 1.802013835206515036E-11, 5.105276777067893512 ) ) ;
#11298 = CARTESIAN_POINT ( 'NONE',  ( 52.29715082351538769, 52.60051614449766788, -6.992620115222796251 ) ) ;
#11299 = CARTESIAN_POINT ( 'NONE',  ( 53.50833635130540955, 51.69948385550241454, -4.867452303228209765 ) ) ;
#11300 = DIRECTION ( 'NONE',  ( 0.000000000000000000, -0.000000000000000000, -1.000000000000000000 ) ) ;
#11301 = ORIENTED_EDGE ( 'NONE', *, *, #8568, .T. ) ;
#11302 = CIRCLE ( 'NONE', #2472, 2.100000000000000089 ) ;
#11303 = AXIS2_PLACEMENT_3D ( 'NONE', #9018, #13214, #3833 ) ;
#11304 = AXIS2_PLACEMENT_3D ( 'NONE', #8752, #7716, #173 ) ;
#11305 = VERTEX_POINT ( 'NONE', #5501 ) ;
#11306 = ORIENTED_EDGE ( 'NONE', *, *, #11225, .F. ) ;
#11307 = CARTESIAN_POINT ( 'NONE',  ( -1.000000000000000000, -14.00000000000000000, -9.000000000000001776 ) ) ;
#11308 = DIRECTION ( 'NONE',  ( 1.000000000000000000, -6.938893903907227392E-16, 0.000000000000000000 ) ) ;
#11309 = DIRECTION ( 'NONE',  ( 0.03086419753086420623, 0.9995235871707959241, -0.000000000000000000 ) ) ;
#11310 = CARTESIAN_POINT ( 'NONE',  ( 45.86712807150323812, 47.29948385550240886, -5.649768623646098220 ) ) ;
#11311 = SURFACE_STYLE_FILL_AREA ( #2880 ) ;
#11312 = CARTESIAN_POINT ( 'NONE',  ( 6.327625087026996553, 2.033113452595566972, -4.999999999998725464 ) ) ;
#11313 = CARTESIAN_POINT ( 'NONE',  ( 50.02271294988511841, 64.49948385550239038, 6.000000000000000888 ) ) ;
#11314 = DIRECTION ( 'NONE',  ( 0.000000000000000000, -0.000000000000000000, 1.000000000000000000 ) ) ;
#11315 = CARTESIAN_POINT ( 'NONE',  ( 57.36023556966787851, 55.99948385550239038, -0.02388180880522424582 ) ) ;
#11316 = CARTESIAN_POINT ( 'NONE',  ( 56.65037692655918988, 53.89948385550240317, -2.184720259617163762 ) ) ;
#11317 = ORIENTED_EDGE ( 'NONE', *, *, #10572, .T. ) ;
#11318 = CARTESIAN_POINT ( 'NONE',  ( 54.09612160359786515, 51.69948385550240744, -5.676469297603166098 ) ) ;
#11319 = VERTEX_POINT ( 'NONE', #7379 ) ;
#11320 = CARTESIAN_POINT ( 'NONE',  ( 3.948095570617042860, 0.6965071952218068185, 3.500000000000155875 ) ) ;
#11321 = ORIENTED_EDGE ( 'NONE', *, *, #2783, .F. ) ;
#11322 = EDGE_CURVE ( 'NONE', #10955, #11356, #12562, .T. ) ;
#11323 = CARTESIAN_POINT ( 'NONE',  ( 20.00000000000000000, -25.00000000000000711, -20.00000000000000000 ) ) ;
#11324 = AXIS2_PLACEMENT_3D ( 'NONE', #7127, #3868, #1785 ) ;
#11325 = DIRECTION ( 'NONE',  ( 1.000000000000000000, 0.000000000000000000, 0.000000000000000000 ) ) ;
#11326 = CARTESIAN_POINT ( 'NONE',  ( 6.367873360227559232, -5.773502691896263528, 0.000000000000000000 ) ) ;
#11327 = CARTESIAN_POINT ( 'NONE',  ( 44.30067958973594955, 60.10051614449766788, -1.875703265242155693 ) ) ;
#11328 = CARTESIAN_POINT ( 'NONE',  ( 0.000000000000000000, 0.000000000000000000, -25.03750572909317285 ) ) ;
#11329 = CARTESIAN_POINT ( 'NONE',  ( 54.68390685589033495, 57.69948385550241454, -6.485486291978119766 ) ) ;
#11330 = CLOSED_SHELL ( 'NONE', ( #4937, #1263, #1013, #3146, #4169, #10022, #395, #13385, #11524, #8255, #10148, #13261, #8879, #11463, #10725, #3150, #9314, #8986, #4390, #446, #10928, #3396, #7684, #8478, #7357, #7557, #9881, #6961, #12795 ) ) ;
#11331 = MECHANICAL_DESIGN_GEOMETRIC_PRESENTATION_REPRESENTATION (  '', ( #70 ), #2268 ) ;
#11332 = CARTESIAN_POINT ( 'NONE',  ( 45.86712807150323812, 65.29948385550241596, -5.649768623646098220 ) ) ;
#11333 = DIRECTION ( 'NONE',  ( -9.858538378746663627E-23, 5.031452844637890958E-23, -1.000000000000000000 ) ) ;
#11334 = EDGE_CURVE ( 'NONE', #3771, #13411, #11525, .T. ) ;
#11335 = B_SPLINE_CURVE_WITH_KNOTS ( 'NONE', 3,
 ( #4769, #8980, #8016, #2685, #11185, #8089, #12225, #12090, #656, #7947, #12295, #13387, #12160, #6025, #13180, #6910 ),
 .UNSPECIFIED., .F., .F.,
 ( 4, 3, 3, 3, 3, 4 ),
 ( -2.669610558406318528E-06, 0.000000000000000000, 5.703179328867203279E-05, 0.0001157653700806028548, 0.0001686517580799736817, 0.0002219032271235106112 ),
 .UNSPECIFIED. ) ;
#11336 = EDGE_CURVE ( 'NONE', #13062, #10104, #8707, .T. ) ;
#11337 = CARTESIAN_POINT ( 'NONE',  ( 45.27934281921075410, 47.29948385550241596, -6.458785618021043895 ) ) ;
#11338 = B_SPLINE_CURVE_WITH_KNOTS ( 'NONE', 3,
 ( #6049, #10517, #8384, #5147, #13549, #12591, #4099, #4934 ),
 .UNSPECIFIED., .F., .F.,
 ( 4, 2, 2, 4 ),
 ( 0.005725059856848645212, 0.006314084072593634418, 0.006903108288338624492, 0.008081156719828603771 ),
 .UNSPECIFIED. ) ;
#11339 = EDGE_CURVE ( 'NONE', #6904, #11968, #3221, .T. ) ;
#11340 = VERTEX_POINT ( 'NONE', #5443 ) ;
#11341 = ORIENTED_EDGE ( 'NONE', *, *, #4336, .F. ) ;
#11342 = EDGE_CURVE ( 'NONE', #10268, #4657, #11676, .T. ) ;
#11343 = VERTEX_POINT ( 'NONE', #4322 ) ;
#11344 = CARTESIAN_POINT ( 'NONE',  ( 2.449293598294706513E-15, -20.00000000000000000, -10.00000000000000000 ) ) ;
#11345 = LINE ( 'NONE', #3878, #1812 ) ;
#11346 = FACE_OUTER_BOUND ( 'NONE', #5906, .T. ) ;
#11347 = DIRECTION ( 'NONE',  ( -1.387778780781445991E-14, 0.000000000000000000, -1.000000000000000000 ) ) ;
#11348 = CARTESIAN_POINT ( 'NONE',  ( 50.02271294988511841, 64.49948385550239038, 6.000000000000000888 ) ) ;
#11349 = CARTESIAN_POINT ( 'NONE',  ( 50.02271294988505446, 52.50051614449765935, -7.000000000000000888 ) ) ;
#11350 = TOROIDAL_SURFACE ( 'NONE', #12663, 5.200000000000001066, 0.4999999999999978351 ) ;
#11351 = CARTESIAN_POINT ( 'NONE',  ( 52.62207051974829852, 60.60051614449765367, -7.992620115222797139 ) ) ;
#11352 = CARTESIAN_POINT ( 'NONE',  ( 3.806834918298644066, -4.553649124439118623E-15, -3.499999999999999556 ) ) ;
#11353 = CARTESIAN_POINT ( 'NONE',  ( 56.81924384183006538, 48.80051614449767072, -4.924951120819380357 ) ) ;
#11355 = VERTEX_POINT ( 'NONE', #8544 ) ;
#11354 = ORIENTED_EDGE ( 'NONE', *, *, #13093, .T. ) ;
#11356 = VERTEX_POINT ( 'NONE', #2233 ) ;
#11357 = EDGE_CURVE ( 'NONE', #1824, #1406, #5502, .T. ) ;
#11358 = PRODUCT_DEFINITION_CONTEXT ( 'detailed design', #2124, 'design' ) ;
#11359 = VERTEX_POINT ( 'NONE', #7505 ) ;
#11360 = AXIS2_PLACEMENT_3D ( 'NONE', #365, #10874, #9010 ) ;
#11361 = CARTESIAN_POINT ( 'NONE',  ( -1.240299975428113101E-15, -4.647091401871173311, -3.572172305156514849 ) ) ;
#11362 = CARTESIAN_POINT ( 'NONE',  ( 0.1983443223721567394, 3.359771601077105707, -4.180704885107416224 ) ) ;
#11363 = VECTOR ( 'NONE', #10677, 1000.000000000000000 ) ;
#11364 = DIRECTION ( 'NONE',  ( -0.000000000000000000, -0.000000000000000000, 1.000000000000000000 ) ) ;
#11365 = APPLICATION_PROTOCOL_DEFINITION ( 'draft international standard', 'automotive_design', 1998, #5673 ) ;
#11366 = CARTESIAN_POINT ( 'NONE',  ( 42.63976443033212860, 60.99948385550238328, 0.02388180880522514787 ) ) ;
#11367 = CARTESIAN_POINT ( 'NONE',  ( 55.96859303347805081, 58.19948385550240744, 4.306917132069425058 ) ) ;
#11368 = CIRCLE ( 'NONE', #7609, 5.000000000000000000 ) ;
#11369 = DIRECTION ( 'NONE',  ( 0.000000000000000000, -1.224646799147353947E-16, 1.000000000000000000 ) ) ;
#11370 = CONICAL_SURFACE ( 'NONE', #8292, 3.500000000000000000, 1.047197551196600296 ) ;
#11371 = DIRECTION ( 'NONE',  ( 0.000000000000000000, 0.000000000000000000, -1.000000000000000000 ) ) ;
#11372 = CARTESIAN_POINT ( 'NONE',  ( 51.03999344061968912, 45.00000000000002132, -7.500000000000003553 ) ) ;
#11373 = CARTESIAN_POINT ( 'NONE',  ( 44.03140696652198471, 47.80051614449764230, 4.306917132069485454 ) ) ;
#11374 = CARTESIAN_POINT ( 'NONE',  ( 49.97728705011488870, 55.49948385550241170, -6.000000000000000888 ) ) ;
#11375 = DIRECTION ( 'NONE',  ( -0.000000000000000000, -0.000000000000000000, -1.000000000000000000 ) ) ;
#11376 = EDGE_LOOP ( 'NONE', ( #13362, #7313, #50, #9594 ) ) ;
#11377 = ADVANCED_FACE ( 'NONE', ( #10681 ), #9642, .F. ) ;
#11378 = CARTESIAN_POINT ( 'NONE',  ( 14.14213562373095101, -25.00000000000000711, -20.00000000000000000 ) ) ;
#11379 = ORIENTED_EDGE ( 'NONE', *, *, #3933, .T. ) ;
#11380 = EDGE_LOOP ( 'NONE', ( #665, #7959, #9329, #6936 ) ) ;
#11381 = DIRECTION ( 'NONE',  ( 0.000000000000000000, 0.000000000000000000, 1.000000000000000000 ) ) ;
#11382 = PLANE ( 'NONE',  #7822 ) ;
#11383 = CIRCLE ( 'NONE', #9175, 12.49999999999999645 ) ;
#11384 = CYLINDRICAL_SURFACE ( 'NONE', #13477, 0.7500000000000000000 ) ;
#11385 = CARTESIAN_POINT ( 'NONE',  ( 4.200000000000001954, 2.449293598294707893E-16, -2.000000000000000888 ) ) ;
#11386 = DIRECTION ( 'NONE',  ( 0.000000000000000000, 0.000000000000000000, 1.000000000000000000 ) ) ;
#11387 = CARTESIAN_POINT ( 'NONE',  ( 55.69932041026404335, 63.89948385550240317, -1.875703265242203432 ) ) ;
#11388 = CARTESIAN_POINT ( 'NONE',  ( 0.2175679805410235534, -1.691499766303381058, -3.499999999999999556 ) ) ;
#11389 = CARTESIAN_POINT ( 'NONE',  ( 42.63976443033212860, 56.99948385550241170, 0.02388180880522514787 ) ) ;
#11390 = CARTESIAN_POINT ( 'NONE',  ( 43.34962307344081012, 54.89948385550240317, 2.184720259617164650 ) ) ;
#11391 = VERTEX_POINT ( 'NONE', #10742 ) ;
#11392 = CARTESIAN_POINT ( 'NONE',  ( 44.03140696652192787, 49.19948385550240033, -4.306917132069425058 ) ) ;
#11393 = ORIENTED_EDGE ( 'NONE', *, *, #8779, .T. ) ;
#11394 = CARTESIAN_POINT ( 'NONE',  ( 4.086262418390198548, -2.102635014057361751, 3.500000000000000444 ) ) ;
#11395 = ORIENTED_EDGE ( 'NONE', *, *, #3811, .F. ) ;
#11396 = CARTESIAN_POINT ( 'NONE',  ( 20.00000000000000000, -20.00000000000000000, -20.00000000000000000 ) ) ;
#11397 = CARTESIAN_POINT ( 'NONE',  ( 4.050823680195226650, -3.779313952391382792, 0.5899027668435167238 ) ) ;
#11398 = CARTESIAN_POINT ( 'NONE',  ( 54.13287192849676188, 48.29948385550240175, 5.649768623646098220 ) ) ;
#11399 = AXIS2_PLACEMENT_3D ( 'NONE', #5434, #357, #6667 ) ;
#11400 = CARTESIAN_POINT ( 'NONE',  ( 55.69932041026405045, 59.10051614449766078, 1.875703265242156359 ) ) ;
#11401 = PRODUCT ( 'circlip for shafts normal_din_Circlip DIN 471 - 10 x 1', 'circlip for shafts normal_din_Circlip DIN 471 - 10 x 1', '', ( #8191 ) ) ;
#11402 = CARTESIAN_POINT ( 'NONE',  ( -4.000000000000000000, 0.7924765000094600165, -0.05906175389889745803 ) ) ;
#11403 = CARTESIAN_POINT ( 'NONE',  ( 57.60143344285433642, 61.89948385550241738, -2.493737253992118319 ) ) ;
#11404 = DIRECTION ( 'NONE',  ( -9.251858538542972814E-17, -1.000000000000000000, 0.000000000000000000 ) ) ;
#11405 = EDGE_CURVE ( 'NONE', #6039, #4300, #1250, .T. ) ;
#11406 = CARTESIAN_POINT ( 'NONE',  ( 50.02271294988513972, 52.49948385550241170, 8.000000000000001776 ) ) ;
#11407 = ORIENTED_EDGE ( 'NONE', *, *, #4819, .T. ) ;
#11408 = VERTEX_POINT ( 'NONE', #7777 ) ;
#11409 = ORIENTED_EDGE ( 'NONE', *, *, #4404, .T. ) ;
#11410 = DIRECTION ( 'NONE',  ( -1.000000000000000000, -0.000000000000000000, -0.000000000000000000 ) ) ;
#11411 = SURFACE_SIDE_STYLE ('',( #12442 ) ) ;
#11412 = DIRECTION ( 'NONE',  ( -1.000000000000000000, -0.000000000000000000, -0.000000000000000000 ) ) ;
#11413 = CARTESIAN_POINT ( 'NONE',  ( -1.655952806101422814, 3.662737355149034979, -7.623296525288699970E-18 ) ) ;
#11414 = DIRECTION ( 'NONE',  ( 0.000000000000000000, 1.000000000000000000, 0.000000000000000000 ) ) ;
#11415 = CARTESIAN_POINT ( 'NONE',  ( 55.08986747509847248, 63.79948385550241596, -3.727524721679197572 ) ) ;
#11416 = CARTESIAN_POINT ( 'NONE',  ( 52.29715082351539479, 56.60051614449766078, -6.992620115222796251 ) ) ;
#11417 = CARTESIAN_POINT ( 'NONE',  ( 47.42335538002180328, 58.40051614449765793, -8.007379884777206414 ) ) ;
#11418 = DIRECTION ( 'NONE',  ( 1.000000000000000000, 0.000000000000000000, 0.000000000000000000 ) ) ;
#11419 = CARTESIAN_POINT ( 'NONE',  ( 42.39856655714564226, 52.10051614449766788, -2.493737253992044156 ) ) ;
#11421 = ORIENTED_EDGE ( 'NONE', *, *, #13481, .T. ) ;
#11420 = ORIENTED_EDGE ( 'NONE', *, *, #7876, .F. ) ;
#11422 = ORIENTED_EDGE ( 'NONE', *, *, #11521, .F. ) ;
#11423 = EDGE_LOOP ( 'NONE', ( #537, #6263 ) ) ;
#11424 = DIRECTION ( 'NONE',  ( -0.000000000000000000, -0.000000000000000000, -1.000000000000000000 ) ) ;
#11425 = CYLINDRICAL_SURFACE ( 'NONE', #3703, 12.50000000000000000 ) ;
#11426 = DIRECTION ( 'NONE',  ( 0.000000000000000000, 0.000000000000000000, 1.000000000000000000 ) ) ;
#11427 = DIRECTION ( 'NONE',  ( -1.000000000000000000, 0.000000000000000000, 0.000000000000000000 ) ) ;
#11428 = CONTEXT_DEPENDENT_SHAPE_REPRESENTATION ( #4514, #5684 ) ;
#11429 = CARTESIAN_POINT ( 'NONE',  ( 56.66441430157296821, 62.09948385550239891, 2.141517661632100111 ) ) ;
#11430 = CARTESIAN_POINT ( 'NONE',  ( 57.36023556966787851, 61.99948385550240459, -0.02388180880522424582 ) ) ;
#11431 = ADVANCED_FACE ( 'NONE', ( #10091 ), #6992, .F. ) ;
#11432 = CARTESIAN_POINT ( 'NONE',  ( 56.65037692655921120, 59.10051614449766078, 2.184720259617097593 ) ) ;
#11433 = EDGE_CURVE ( 'NONE', #4979, #8761, #8029, .T. ) ;
#11434 =( GEOMETRIC_REPRESENTATION_CONTEXT ( 3 ) GLOBAL_UNCERTAINTY_ASSIGNED_CONTEXT ( ( #6495 ) ) GLOBAL_UNIT_ASSIGNED_CONTEXT ( ( #3267, #9291, #4035 ) ) REPRESENTATION_CONTEXT ( 'NONE', 'WORKASPACE' ) );
#11435 = CARTESIAN_POINT ( 'NONE',  ( -14.99999999999999822, -19.99999999999999645, -50.00000000000000000 ) ) ;
#11436 = CYLINDRICAL_SURFACE ( 'NONE', #2555, 5.000000000000000888 ) ;
#11437 = CARTESIAN_POINT ( 'NONE',  ( 55.31939397794342028, 44.99999999999998579, -5.196074157289758411 ) ) ;
#11438 = CARTESIAN_POINT ( 'NONE',  ( 56.65037692655921120, 49.10051614449766078, 2.184720259617097593 ) ) ;
#11439 = CARTESIAN_POINT ( 'NONE',  ( 44.91013252490152752, 50.79948385550240175, 3.727524721679198461 ) ) ;
#11440 = DIRECTION ( 'NONE',  ( -9.858538378746663627E-23, 5.031452844637890958E-23, -1.000000000000000000 ) ) ;
#11441 = EDGE_CURVE ( 'NONE', #12021, #9971, #4850, .T. ) ;
#11442 = ORIENTED_EDGE ( 'NONE', *, *, #11069, .T. ) ;
#11443 = CARTESIAN_POINT ( 'NONE',  ( -5.686050877451574337, -5.768780236673276995, 0.000000000000000000 ) ) ;
#11444 = ORIENTED_EDGE ( 'NONE', *, *, #5014, .F. ) ;
#11445 = ORIENTED_EDGE ( 'NONE', *, *, #4834, .F. ) ;
#11446 = CARTESIAN_POINT ( 'NONE',  ( 4.124214193018069352, -2.028338413290947440, -3.513185186763551737 ) ) ;
#11447 = CIRCLE ( 'NONE', #8799, 4.000000000000003553 ) ;
#11448 = CARTESIAN_POINT ( 'NONE',  ( 0.000000000000000000, 0.000000000000000000, 10.00000000000000000 ) ) ;
#11449 = CARTESIAN_POINT ( 'NONE',  ( -74.99999999999997158, -39.99999999999998579, 10.00000000000000000 ) ) ;
#11450 = SURFACE_STYLE_FILL_AREA ( #12555 ) ;
#11451 = DIRECTION ( 'NONE',  ( 1.000000000000000000, 0.000000000000000000, 0.000000000000000000 ) ) ;
#11452 = CARTESIAN_POINT ( 'NONE',  ( 75.00000000000001421, -7.499999999999971578, -10.00000000000000000 ) ) ;
#11453 = CARTESIAN_POINT ( 'NONE',  ( 49.97728705011494554, 47.50051614449765935, 6.000000000000000888 ) ) ;
#11454 = DIRECTION ( 'NONE',  ( 0.000000000000000000, 0.000000000000000000, 1.000000000000000000 ) ) ;
#11455 = CARTESIAN_POINT ( 'NONE',  ( 49.97728705011488159, 63.49948385550241170, -7.000000000000000888 ) ) ;
#11456 = CARTESIAN_POINT ( 'NONE',  ( 47.74827507625478518, 56.59948385550238470, 7.007379884777227730 ) ) ;
#11457 = CIRCLE ( 'NONE', #10350, 0.7499999999999997780 ) ;
#11458 = ORIENTED_EDGE ( 'NONE', *, *, #7795, .F. ) ;
#11459 = CARTESIAN_POINT ( 'NONE',  ( 42.63976443033212860, 52.99948385550240459, 0.02388180880522514787 ) ) ;
#11460 = AXIS2_PLACEMENT_3D ( 'NONE', #7054, #11265, #3431 ) ;
#11461 = EDGE_LOOP ( 'NONE', ( #12138, #8994, #6249, #13538 ) ) ;
#11462 = CARTESIAN_POINT ( 'NONE',  ( -62.49999999999997158, 32.50000000000001421, -10.00000000000000178 ) ) ;
#11463 = ADVANCED_FACE ( 'NONE', ( #5637 ), #8156, .T. ) ;
#11464 = ORIENTED_EDGE ( 'NONE', *, *, #1729, .T. ) ;
#11465 = DIRECTION ( 'NONE',  ( 0.000000000000000000, 0.000000000000000000, 1.000000000000000000 ) ) ;
#11466 =( GEOMETRIC_REPRESENTATION_CONTEXT ( 3 ) GLOBAL_UNCERTAINTY_ASSIGNED_CONTEXT ( ( #4675 ) ) GLOBAL_UNIT_ASSIGNED_CONTEXT ( ( #9384, #3087, #3019 ) ) REPRESENTATION_CONTEXT ( 'NONE', 'WORKASPACE' ) );
#11467 = AXIS2_PLACEMENT_3D ( 'NONE', #5566, #4524, #13465 ) ;
#11468 = DIRECTION ( 'NONE',  ( -1.000000000000000000, -0.000000000000000000, -0.000000000000000000 ) ) ;
#11469 = CARTESIAN_POINT ( 'NONE',  ( 52.25172492374522903, 45.59948385550240602, -7.007379884777227730 ) ) ;
#11470 = CARTESIAN_POINT ( 'NONE',  ( 52.29715082351538769, 46.60051614449766078, -6.992620115222796251 ) ) ;
#11471 = CIRCLE ( 'NONE', #850, 5.000000000000000888 ) ;
#11472 = DIRECTION ( 'NONE',  ( 1.000000000000000000, 0.000000000000000000, 0.000000000000000000 ) ) ;
#11473 = EDGE_CURVE ( 'NONE', #12675, #10104, #11232, .T. ) ;
#11474 = EDGE_CURVE ( 'NONE', #10246, #8295, #4396, .T. ) ;
#11475 = CARTESIAN_POINT ( 'NONE',  ( 56.66441430157296821, 48.09948385550240602, 2.141517661632100111 ) ) ;
#11476 = LINE ( 'NONE', #1658, #2462 ) ;
#11477 = CARTESIAN_POINT ( 'NONE',  ( 1.925929944387235853E-31, 15.00000000000001599, -15.00000000000000000 ) ) ;
#11478 = CARTESIAN_POINT ( 'NONE',  ( 58.41169779390614281, 47.99948385550239038, -0.02388180880523160798 ) ) ;
#11479 = CIRCLE ( 'NONE', #13006, 4.800000000000000711 ) ;
#11480 = ORIENTED_EDGE ( 'NONE', *, *, #7579, .F. ) ;
#11481 = ORIENTED_EDGE ( 'NONE', *, *, #10570, .T. ) ;
#11482 = ORIENTED_EDGE ( 'NONE', *, *, #12275, .T. ) ;
#11483 = CARTESIAN_POINT ( 'NONE',  ( 54.65205120807737416, 44.75923773080658918, -4.999999999999772626 ) ) ;
#11484 = PRODUCT_DEFINITION ( 'UNKNOWN', '', #7065, #11022 ) ;
#11485 = SURFACE_STYLE_USAGE ( .BOTH. , #11411 ) ;
#11486 = DIRECTION ( 'NONE',  ( 0.000000000000000000, 0.000000000000000000, 1.000000000000000000 ) ) ;
#11487 = CARTESIAN_POINT ( 'NONE',  ( -0.3208286057739654917, 4.433571671609680465, -0.3503314178412548774 ) ) ;
#11488 = PRESENTATION_LAYER_ASSIGNMENT (  '', '', ( #10377 ) ) ;
#11489 = CARTESIAN_POINT ( 'NONE',  ( 3.472371940585993855, 2.614027278893175321, -3.320322319201766792 ) ) ;
#11490 = VECTOR ( 'NONE', #11549, 1000.000000000000000 ) ;
#11491 = CARTESIAN_POINT ( 'NONE',  ( 53.50833635130544508, 51.30051614449765651, 4.867452303228181343 ) ) ;
#11492 = CARTESIAN_POINT ( 'NONE',  ( 43.33558569842706021, 57.90051614449766504, 2.141517661632167169 ) ) ;
#11493 = CARTESIAN_POINT ( 'NONE',  ( 54.72065718078918906, 60.70051614449766930, -6.458785618021089192 ) ) ;
#11494 = CARTESIAN_POINT ( 'NONE',  ( -4.000000000000000000, -0.8232339106130515116, -3.430630286862743183 ) ) ;
#11495 = CARTESIAN_POINT ( 'NONE',  ( 54.68390685589039890, 47.30051614449766362, 6.485486291978072693 ) ) ;
#11497 = ORIENTED_EDGE ( 'NONE', *, *, #12407, .F. ) ;
#11496 = ORIENTED_EDGE ( 'NONE', *, *, #7224, .F. ) ;
#11498 =( BOUNDED_SURFACE ( )  B_SPLINE_SURFACE ( 3, 2, ( 
 ( #1269, #7523, #11606 ),
 ( #2250, #7594, #10629 ),
 ( #2184, #12633, #6429 ),
 ( #12826, #119, #5319 ),
 ( #1068, #11798, #5255 ),
 ( #5517, #248, #10557 ) ),
 .UNSPECIFIED., .F., .F., .F. ) 
 B_SPLINE_SURFACE_WITH_KNOTS ( ( 4, 2, 4 ),
 ( 3, 3 ),
 ( 0.02032853247518126918, 0.02278863295364821906, 0.02524873343211516893 ),
 ( 0.000000000000000000, 1.000000000000000000 ),
 .UNSPECIFIED. ) 
 GEOMETRIC_REPRESENTATION_ITEM ( )  RATIONAL_B_SPLINE_SURFACE ( (
 ( 1.000000000000000000, 0.8047781615896838492, 1.000000000000000000),
 ( 1.000000000000000000, 0.8123767586288186404, 1.000000000000000000),
 ( 1.000000000000000000, 0.8190662415565814758, 1.000000000000000000),
 ( 1.000000000000000000, 0.8192361015667604107, 1.000000000000000000),
 ( 1.000000000000000000, 0.8126135807104967190, 1.000000000000000000),
 ( 1.000000000000000000, 0.8047712338318580017, 1.000000000000000000) ) ) 
 REPRESENTATION_ITEM ( '' )  SURFACE ( )  );
#11499 = ORIENTED_EDGE ( 'NONE', *, *, #10231, .T. ) ;
#11500 = UNCERTAINTY_MEASURE_WITH_UNIT (LENGTH_MEASURE( 1.000000000000000082E-05 ), #13300, 'distance_accuracy_value', 'NONE');
#11501 = ORIENTED_EDGE ( 'NONE', *, *, #22, .T. ) ;
#11502 = AXIS2_PLACEMENT_3D ( 'NONE', #9693, #3404, #3813 ) ;
#11503 = CARTESIAN_POINT ( 'NONE',  ( 49.99999999999997158, 45.00000000000003553, -7.000000000000000888 ) ) ;
#11504 = CARTESIAN_POINT ( 'NONE',  ( 1.925929944387235853E-31, 15.00000000000001599, -9.000000000000000000 ) ) ;
#11505 = EDGE_CURVE ( 'NONE', #7289, #4363, #4914, .T. ) ;
#11506 = CARTESIAN_POINT ( 'NONE',  ( 0.000000000000000000, 1.773042676681340524, -2.059984127722458425E-15 ) ) ;
#11507 = DIRECTION ( 'NONE',  ( 0.000000000000000000, 0.000000000000000000, -1.000000000000000000 ) ) ;
#11508 = CARTESIAN_POINT ( 'NONE',  ( 45.86712807150323812, 61.29948385550240886, -5.649768623646098220 ) ) ;
#11509 = DIRECTION ( 'NONE',  ( -1.000000000000000000, 0.000000000000000000, 0.000000000000000000 ) ) ;
#11510 = CARTESIAN_POINT ( 'NONE',  ( 50.02271294988505446, 62.50051614449766646, -7.000000000000000888 ) ) ;
#11511 = AXIS2_PLACEMENT_3D ( 'NONE', #11771, #6532, #3136 ) ;
#11512 = CARTESIAN_POINT ( 'NONE',  ( 2.000000000000000000, 1.773042676681340524, -2.059984127722458425E-15 ) ) ;
#11513 = CARTESIAN_POINT ( 'NONE',  ( -0.2500000000000000000, -8.096141056083446585, 0.000000000000000000 ) ) ;
#11514 = CARTESIAN_POINT ( 'NONE',  ( 4.158806965674307854, 4.075748668183981849, 0.05940377217583739378 ) ) ;
#11515 = CARTESIAN_POINT ( 'NONE',  ( 44.05948171654945611, 50.20051614449764088, -4.345558710429044069 ) ) ;
#11516 = CARTESIAN_POINT ( 'NONE',  ( 56.30877334542961421, 61.99948385550241170, -0.02388180880520959434 ) ) ;
#11517 = DIRECTION ( 'NONE',  ( 9.858538378746663627E-23, -5.031452844637890958E-23, 1.000000000000000000 ) ) ;
#11518 = ADVANCED_FACE ( 'NONE', ( #8678 ), #608, .T. ) ;
#11519 = ORIENTED_EDGE ( 'NONE', *, *, #12694, .F. ) ;
#11520 = DIRECTION ( 'NONE',  ( 1.000000000000000000, 0.000000000000000000, 0.000000000000000000 ) ) ;
#11521 = EDGE_CURVE ( 'NONE', #11042, #13345, #4251, .T. ) ;
#11522 = ORIENTED_EDGE ( 'NONE', *, *, #7391, .T. ) ;
#11524 = ADVANCED_FACE ( 'NONE', ( #13010 ), #10574, .T. ) ;
#11523 = ORIENTED_EDGE ( 'NONE', *, *, #1344, .F. ) ;
#11525 = LINE ( 'NONE', #2166, #6401 ) ;
#11526 = AXIS2_PLACEMENT_3D ( 'NONE', #9733, #9458, #11663 ) ;
#11527 = EDGE_CURVE ( 'NONE', #10855, #5998, #4590, .T. ) ;
#11528 = CARTESIAN_POINT ( 'NONE',  ( -6.080745460913608902, 0.5192545390863924082, -1.000000000000000000 ) ) ;
#11529 = DIRECTION ( 'NONE',  ( 1.000000000000000000, 0.000000000000000000, 0.000000000000000000 ) ) ;
#11530 = LINE ( 'NONE', #13507, #833 ) ;
#11531 = EDGE_CURVE ( 'NONE', #5893, #10938, #1968, .T. ) ;
#11532 = CARTESIAN_POINT ( 'NONE',  ( 1.000000000000002442, -20.00000000000000000, -9.000000000000001776 ) ) ;
#11533 = CARTESIAN_POINT ( 'NONE',  ( 53.54508667620424234, 50.70051614449766220, -4.840751629271188961 ) ) ;
#11534 = CARTESIAN_POINT ( 'NONE',  ( -74.99999999999997158, -39.99999999999998579, 10.00000000000000000 ) ) ;
#11535 = CARTESIAN_POINT ( 'NONE',  ( 47.74827507625478518, 64.59948385550239891, 7.007379884777227730 ) ) ;
#11536 = CARTESIAN_POINT ( 'NONE',  ( 52.25172492374522903, 55.59948385550241312, -7.007379884777225953 ) ) ;
#11537 = VECTOR ( 'NONE', #11721, 1000.000000000000000 ) ;
#11538 = ORIENTED_EDGE ( 'NONE', *, *, #12746, .T. ) ;
#11539 = ORIENTED_EDGE ( 'NONE', *, *, #10428, .T. ) ;
#11540 = EDGE_CURVE ( 'NONE', #11760, #12920, #743, .T. ) ;
#11541 = DIRECTION ( 'NONE',  ( 1.000000000000000000, 0.000000000000000000, 0.000000000000000000 ) ) ;
#11542 = EDGE_CURVE ( 'NONE', #13537, #2771, #8809, .T. ) ;
#11543 = CARTESIAN_POINT ( 'NONE',  ( 5.686050877451574337, -5.768780236673276995, -1.000000000000000000 ) ) ;
#11544 = DIRECTION ( 'NONE',  ( -1.000000000000000000, 0.000000000000000000, -0.000000000000000000 ) ) ;
#11545 = AXIS2_PLACEMENT_3D ( 'NONE', #8313, #5338, #9414 ) ;
#11546 = DIRECTION ( 'NONE',  ( 0.000000000000000000, 0.000000000000000000, 1.000000000000000000 ) ) ;
#11547 = CARTESIAN_POINT ( 'NONE',  ( 49.97728705011488159, 47.49948385550240459, -7.000000000000000888 ) ) ;
#11548 = CARTESIAN_POINT ( 'NONE',  ( 44.05948171654945611, 46.20051614449766930, -4.345558710429044069 ) ) ;
#11549 = DIRECTION ( 'NONE',  ( 0.000000000000000000, -0.000000000000000000, -1.000000000000000000 ) ) ;
#11550 = CARTESIAN_POINT ( 'NONE',  ( 42.63976443033212860, 46.99948385550240459, 0.02388180880522514787 ) ) ;
#11551 =( NAMED_UNIT ( * ) SI_UNIT ( $, .STERADIAN. ) SOLID_ANGLE_UNIT ( ) );
#11552 = CARTESIAN_POINT ( 'NONE',  ( 52.57664461997811856, 57.59948385550240602, -8.007379884777229506 ) ) ;
#11553 = EDGE_LOOP ( 'NONE', ( #868, #9955, #8357 ) ) ;
#11554 = AXIS2_PLACEMENT_3D ( 'NONE', #9551, #9618, #1298 ) ;
#11555 = VERTEX_POINT ( 'NONE', #5965 ) ;
#11556 = EDGE_CURVE ( 'NONE', #2470, #5544, #10989, .T. ) ;
#11557 = DIRECTION ( 'NONE',  ( 0.000000000000000000, 0.000000000000000000, -1.000000000000000000 ) ) ;
#11558 = AXIS2_PLACEMENT_3D ( 'NONE', #12923, #3536, #12994 ) ;
#11559 = PRESENTATION_STYLE_ASSIGNMENT (( #5588 ) ) ;
#11560 = LINE ( 'NONE', #2070, #470 ) ;
#11561 = CARTESIAN_POINT ( 'NONE',  ( 6.092449800118089343, -3.827241605636891641, 3.371023086195408247 ) ) ;
#11562 = CARTESIAN_POINT ( 'NONE',  ( 4.175002511812151873, 2.208363329454889445, -3.469254087858244073 ) ) ;
#11563 = CARTESIAN_POINT ( 'NONE',  ( 49.97728705011494554, 47.50051614449765935, 6.000000000000000888 ) ) ;
#11564 = CARTESIAN_POINT ( 'NONE',  ( 55.96859303347802239, 62.80051614449766362, -4.306917132069484566 ) ) ;
#11565 = CARTESIAN_POINT ( 'NONE',  ( 57.61547081786812896, 48.09948385550240602, 2.450534656007040901 ) ) ;
#11566 = CARTESIAN_POINT ( 'NONE',  ( -4.000000000000000000, 2.471528634177585282, -3.686887442155186712 ) ) ;
#11567 = CARTESIAN_POINT ( 'NONE',  ( 43.18075615816994173, 53.80051614449766362, 4.924951120819380357 ) ) ;
#11568 = ORIENTED_EDGE ( 'NONE', *, *, #10663, .T. ) ;
#11569 = ORIENTED_EDGE ( 'NONE', *, *, #1702, .T. ) ;
#11570 = ORIENTED_EDGE ( 'NONE', *, *, #8717, .F. ) ;
#11571 = CARTESIAN_POINT ( 'NONE',  ( 0.000000000000000000, 0.000000000000000000, 9.999999999999998224 ) ) ;
#11572 = CARTESIAN_POINT ( 'NONE',  ( 6.506987859255528583, 2.925375531177297095, -5.066899051217877314 ) ) ;
#11573 = DIRECTION ( 'NONE',  ( -0.000000000000000000, -1.000000000000000000, -0.000000000000000000 ) ) ;
#11574 = CARTESIAN_POINT ( 'NONE',  ( 0.000000000000000000, 0.000000000000000000, -4.694516984716113228 ) ) ;
#11575 = CARTESIAN_POINT ( 'NONE',  ( 46.49166364869460466, 48.69948385550241454, 4.867452303228209765 ) ) ;
#11576 = CARTESIAN_POINT ( 'NONE',  ( 45.90387839640214196, 64.69948385550240744, 5.676469297603166098 ) ) ;
#11577 = EDGE_CURVE ( 'NONE', #12805, #8657, #3728, .T. ) ;
#11578 = CARTESIAN_POINT ( 'NONE',  ( 56.81924384183006538, 44.80051614449766362, -4.924951120819380357 ) ) ;
#11579 = CARTESIAN_POINT ( 'NONE',  ( 6.534838248920896930, -2.951765777552406878, 5.112608298763836601 ) ) ;
#11580 = DIRECTION ( 'NONE',  ( 1.000000000000000000, 0.000000000000000000, 0.000000000000000000 ) ) ;
#11581 = CARTESIAN_POINT ( 'NONE',  ( 3.878096787214415642, 2.680238624820947990, -2.357690525401575421 ) ) ;
#11582 = CARTESIAN_POINT ( 'NONE',  ( 52.25172492374527877, 51.40051614449767214, 7.007379884777203749 ) ) ;
#11583 = CARTESIAN_POINT ( 'NONE',  ( 48.07319477248768180, 56.59948385550239891, 6.007379884777225953 ) ) ;
#11584 = CARTESIAN_POINT ( 'NONE',  ( -1.000000000000000000, -14.00000000000000000, 8.999999999999998224 ) ) ;
#11585 = AXIS2_PLACEMENT_3D ( 'NONE', #8119, #1739, #12322 ) ;
#11586 = ORIENTED_EDGE ( 'NONE', *, *, #6378, .F. ) ;
#11587 = DIRECTION ( 'NONE',  ( 0.000000000000000000, 0.000000000000000000, -1.000000000000000000 ) ) ;
#11588 = AXIS2_PLACEMENT_3D ( 'NONE', #3767, #6881, #12068 ) ;
#11589 = ORIENTED_EDGE ( 'NONE', *, *, #11556, .F. ) ;
#11590 = DIRECTION ( 'NONE',  ( 0.000000000000000000, 0.000000000000000000, 1.000000000000000000 ) ) ;
#11591 = DIRECTION ( 'NONE',  ( -0.8191520442889902442, 0.000000000000000000, -0.5735764363510482688 ) ) ;
#11592 = AXIS2_PLACEMENT_3D ( 'NONE', #3442, #2121, #7664 ) ;
#11593 = LINE ( 'NONE', #7575, #11727 ) ;
#11594 = CARTESIAN_POINT ( 'NONE',  ( 55.96859303347804371, 50.19948385550240744, 4.306917132069425946 ) ) ;
#11595 = FACE_OUTER_BOUND ( 'NONE', #11970, .T. ) ;
#11596 = CARTESIAN_POINT ( 'NONE',  ( 48.02776887271750184, 49.60051614449766788, 5.992620115222795363 ) ) ;
#11597 = EDGE_CURVE ( 'NONE', #2116, #3498, #2847, .T. ) ;
#11598 = CARTESIAN_POINT ( 'NONE',  ( 0.000000000000000000, 0.000000000000000000, -4.484454397937119197 ) ) ;
#11599 = VECTOR ( 'NONE', #13306, 1000.000000000000000 ) ;
#11600 = CARTESIAN_POINT ( 'NONE',  ( 0.000000000000000000, 20.00000000000001421, -9.999999999999998224 ) ) ;
#11601 = CARTESIAN_POINT ( 'NONE',  ( 55.96859303347804371, 64.19948385550239323, 4.306917132069425946 ) ) ;
#11602 = CARTESIAN_POINT ( 'NONE',  ( 42.63976443033212860, 58.99948385550239038, 0.02388180880522514787 ) ) ;
#11603 = EDGE_CURVE ( 'NONE', #6246, #2249, #13199, .T. ) ;
#11604 = ORIENTED_EDGE ( 'NONE', *, *, #6846, .F. ) ;
#11605 = ORIENTED_EDGE ( 'NONE', *, *, #11077, .T. ) ;
#11606 = CARTESIAN_POINT ( 'NONE',  ( -4.235886605889389145, -2.417314728048544303, -3.751161874094020909 ) ) ;
#11607 = PLANE ( 'NONE',  #8068 ) ;
#11608 = CARTESIAN_POINT ( 'NONE',  ( 3.950241966888158540, -3.393956070638132871, 1.121495646998118545 ) ) ;
#11609 = FACE_OUTER_BOUND ( 'NONE', #3331, .T. ) ;
#11610 = CARTESIAN_POINT ( 'NONE',  ( 44.03140696652193498, 47.19948385550240744, -4.306917132069424170 ) ) ;
#11611 = CARTESIAN_POINT ( 'NONE',  ( 55.96859303347802239, 46.80051614449767072, -4.306917132069484566 ) ) ;
#11612 = CARTESIAN_POINT ( 'NONE',  ( 0.000000000000000000, 0.000000000000000000, -1.000000000000000000 ) ) ;
#11613 = CARTESIAN_POINT ( 'NONE',  ( 45.31609314410967926, 62.69948385550240744, 6.485486291978119766 ) ) ;
#11614 = CARTESIAN_POINT ( 'NONE',  ( -4.078421086530219064, -3.990950201428956845, -1.000000000000000000 ) ) ;
#11615 = ADVANCED_FACE ( 'NONE', ( #4016 ), #811, .F. ) ;
#11616 = CARTESIAN_POINT ( 'NONE',  ( 41.58830220609386430, 58.99948385550239749, 0.02388180880523263147 ) ) ;
#11617 = ORIENTED_EDGE ( 'NONE', *, *, #8457, .T. ) ;
#11618 = ORIENTED_EDGE ( 'NONE', *, *, #5192, .T. ) ;
#11619 = DIRECTION ( 'NONE',  ( 0.000000000000000000, 1.000000000000000000, 0.000000000000000000 ) ) ;
#11620 = CIRCLE ( 'NONE', #9849, 2.649999999999985700 ) ;
#11621 = CARTESIAN_POINT ( 'NONE',  ( 2.000000000000000000, 0.000000000000000000, 0.000000000000000000 ) ) ;
#11622 = CARTESIAN_POINT ( 'NONE',  ( 6.390820841722131718, -5.837016270311242039, -0.1100087447852515082 ) ) ;
#11623 = LINE ( 'NONE', #8246, #8102 ) ;
#11624 = CARTESIAN_POINT ( 'NONE',  ( 51.92680522751238925, 47.40051614449765793, 6.007379884777208190 ) ) ;
#11625 = CARTESIAN_POINT ( 'NONE',  ( 45.86712807150329496, 59.70051614449766220, 5.649768623646139964 ) ) ;
#11626 = CARTESIAN_POINT ( 'NONE',  ( 52.57664461997811856, 49.59948385550241312, -8.007379884777229506 ) ) ;
#11627 = CARTESIAN_POINT ( 'NONE',  ( 3.958484000407329617, 3.734437307742037415, 0.5317648453100634054 ) ) ;
#11628 = CARTESIAN_POINT ( 'NONE',  ( 54.68390685589039890, 55.30051614449765651, 6.485486291978072693 ) ) ;
#11629 = EDGE_LOOP ( 'NONE', ( #12693, #13347, #10315, #2035 ) ) ;
#11630 = AXIS2_PLACEMENT_3D ( 'NONE', #13266, #4856, #604 ) ;
#11631 = EDGE_LOOP ( 'NONE', ( #6525, #1682, #8521, #922, #12657 ) ) ;
#11632 = EDGE_LOOP ( 'NONE', ( #12038, #10591 ) ) ;
#11633 = CARTESIAN_POINT ( 'NONE',  ( 6.452281807715811723, 5.797857616945992554, -1.918911630784297550E-16 ) ) ;
#11634 = FILL_AREA_STYLE ('',( #3061 ) ) ;
#11635 = DIRECTION ( 'NONE',  ( -0.000000000000000000, 1.000000000000000000, -0.000000000000000000 ) ) ;
#11636 = CYLINDRICAL_SURFACE ( 'NONE', #2023, 15.00000000000000000 ) ;
#11637 = CARTESIAN_POINT ( 'NONE',  ( 55.11794222512601493, 48.19948385550240744, 3.688883143319541702 ) ) ;
#11638 = CARTESIAN_POINT ( 'NONE',  ( 52.25172492374522903, 63.59948385550239180, -7.007379884777227730 ) ) ;
#11639 = CARTESIAN_POINT ( 'NONE',  ( 56.79116909180259398, 45.20051614449766220, 4.963592699178938972 ) ) ;
#11640 = CARTESIAN_POINT ( 'NONE',  ( -20.00000000000000000, -19.99999999999999289, -23.00000000000000000 ) ) ;
#11641 = CARTESIAN_POINT ( 'NONE',  ( 4.630153689607048761, 0.000000000000000000, 0.000000000000000000 ) ) ;
#11642 = CARTESIAN_POINT ( 'NONE',  ( 52.29715082351538769, 56.60051614449766788, -6.992620115222796251 ) ) ;
#11643 = CARTESIAN_POINT ( 'NONE',  ( 48.02776887271745210, 59.39948385550240317, -5.992620115222778487 ) ) ;
#11644 = LINE ( 'NONE', #10539, #11795 ) ;
#11645 = ORIENTED_EDGE ( 'NONE', *, *, #11947, .F. ) ;
#11646 = DIRECTION ( 'NONE',  ( -0.000000000000000000, -0.000000000000000000, -1.000000000000000000 ) ) ;
#11647 = ORIENTED_EDGE ( 'NONE', *, *, #284, .T. ) ;
#11648 = DIRECTION ( 'NONE',  ( 1.000000000000000000, 3.469446951953615175E-16, 0.000000000000000000 ) ) ;
#11649 = EDGE_CURVE ( 'NONE', #9468, #7204, #745, .T. ) ;
#11650 = DIRECTION ( 'NONE',  ( 1.000000000000000000, 0.000000000000000000, 0.000000000000000000 ) ) ;
#11651 = CARTESIAN_POINT ( 'NONE',  ( -4.000000000000000000, -0.3979232138631226823, -3.896351557369779711E-17 ) ) ;
#11652 = CARTESIAN_POINT ( 'NONE',  ( 45.90387839640214196, 50.69948385550240744, 5.676469297603166098 ) ) ;
#11653 = CARTESIAN_POINT ( 'NONE',  ( 2.000000000000000000, 0.8865213383406680414, -1.535500000000000975 ) ) ;
#11654 = CARTESIAN_POINT ( 'NONE',  ( 50.02271294988506156, 50.50051614449765935, -6.000000000000000888 ) ) ;
#11655 = PLANE ( 'NONE',  #6315 ) ;
#11656 = CARTESIAN_POINT ( 'NONE',  ( 43.34962307344081012, 64.89948385550239607, 2.184720259617164650 ) ) ;
#11657 = FACE_OUTER_BOUND ( 'NONE', #3887, .T. ) ;
#11658 = CARTESIAN_POINT ( 'NONE',  ( 55.96859303347804371, 60.19948385550240744, 4.306917132069425946 ) ) ;
#11659 = EDGE_LOOP ( 'NONE', ( #8024, #12220, #2183, #13395, #5078, #12171, #3875, #862, #2277, #51, #6345, #10886, #3367, #1917, #13129, #1003 ) ) ;
#11660 = ORIENTED_EDGE ( 'NONE', *, *, #12917, .T. ) ;
#11661 = DIRECTION ( 'NONE',  ( -0.000000000000000000, 0.000000000000000000, -1.000000000000000000 ) ) ;
#11662 = DIRECTION ( 'NONE',  ( -1.000000000000000000, 0.000000000000000000, 0.000000000000000000 ) ) ;
#11663 = DIRECTION ( 'NONE',  ( -1.000000000000000000, 0.000000000000000000, 0.000000000000000000 ) ) ;
#11664 = DIRECTION ( 'NONE',  ( 0.000000000000000000, 0.000000000000000000, 1.000000000000000000 ) ) ;
#11665 = CARTESIAN_POINT ( 'NONE',  ( 45.86712807150323812, 49.29948385550240175, -5.649768623646098220 ) ) ;
#11666 = CARTESIAN_POINT ( 'NONE',  ( 55.94051828345053679, 45.20051614449764088, 4.345558710429044069 ) ) ;
#11667 = CIRCLE ( 'NONE', #8146, 2.149999999999999023 ) ;
#11668 = CARTESIAN_POINT ( 'NONE',  ( 0.000000000000000000, 0.000000000000000000, 0.000000000000000000 ) ) ;
#11669 = ADVANCED_FACE ( 'NONE', ( #3942 ), #6317, .F. ) ;
#11670 = CARTESIAN_POINT ( 'NONE',  ( 47.37792948025162332, 65.39948385550239607, -7.992620115222770494 ) ) ;
#11671 = AXIS2_PLACEMENT_3D ( 'NONE', #4332, #7516, #5383 ) ;
#11672 = CARTESIAN_POINT ( 'NONE',  ( 8.500000000000000000, 0.000000000000000000, 0.000000000000000000 ) ) ;
#11673 = CARTESIAN_POINT ( 'NONE',  ( 57.60143344285433642, 53.89948385550240317, -2.493737253992118319 ) ) ;
#11674 = ORIENTED_EDGE ( 'NONE', *, *, #12031, .T. ) ;
#11675 = ORIENTED_EDGE ( 'NONE', *, *, #9506, .T. ) ;
#11676 = CIRCLE ( 'NONE', #11891, 15.00000000000000000 ) ;
#11677 = CARTESIAN_POINT ( 'NONE',  ( -0.9999999999999995559, -15.10102051443364246, -8.999999999999998224 ) ) ;
#11678 = EDGE_CURVE ( 'NONE', #7186, #7328, #7206, .T. ) ;
#11679 = AXIS2_PLACEMENT_3D ( 'NONE', #4806, #9020, #10116 ) ;
#11680 = ADVANCED_FACE ( 'NONE', ( #4994 ), #9035, .T. ) ;
#11681 = CARTESIAN_POINT ( 'NONE',  ( 30.00000000000000000, 7.500000000000005329, -10.00000000000000711 ) ) ;
#11682 = CARTESIAN_POINT ( 'NONE',  ( 5.686050877451574337, -5.768780236673276995, 0.000000000000000000 ) ) ;
#11683 = CARTESIAN_POINT ( 'NONE',  ( 44.28664221472221385, 45.90051614449766504, 1.832500667257213722 ) ) ;
#11684 = CARTESIAN_POINT ( 'NONE',  ( 55.96859303347802239, 58.80051614449765651, -4.306917132069484566 ) ) ;
#11685 = COLOUR_RGB ( '',1.000000000000000000, 0.9490196078431372140, 0.9098039215686274384 ) ;
#11686 = CARTESIAN_POINT ( 'NONE',  ( 45.27934281921082516, 63.70051614449766930, 6.458785618021089192 ) ) ;
#11687 = DIRECTION ( 'NONE',  ( 1.000000000000000000, 0.000000000000000000, 0.000000000000000000 ) ) ;
#11688 = CARTESIAN_POINT ( 'NONE',  ( 52.57664461997821093, 55.40051614449767214, 8.007379884777206414 ) ) ;
#11689 = EDGE_LOOP ( 'NONE', ( #7006, #5546, #5239 ) ) ;
#11690 = ORIENTED_EDGE ( 'NONE', *, *, #3106, .F. ) ;
#11691 = VERTEX_POINT ( 'NONE', #6109 ) ;
#11692 = CARTESIAN_POINT ( 'NONE',  ( -74.99999999999997158, 40.00000000000001421, 10.00000000000000000 ) ) ;
#11694 = VECTOR ( 'NONE', #7804, 1000.000000000000000 ) ;
#11693 = SURFACE_SIDE_STYLE ('',( #14 ) ) ;
#11695 = LINE ( 'NONE', #11506, #11799 ) ;
#11696 = DIRECTION ( 'NONE',  ( -1.000000000000000000, -0.000000000000000000, -0.000000000000000000 ) ) ;
#11697 = FILL_AREA_STYLE_COLOUR ( '', #1982 ) ;
#11698 = CARTESIAN_POINT ( 'NONE',  ( 48.07319477248768180, 50.59948385550240602, 6.007379884777225953 ) ) ;
#11699 = CARTESIAN_POINT ( 'NONE',  ( 44.05948171654949874, 64.79948385550240175, 4.345558710429104465 ) ) ;
#11700 = CARTESIAN_POINT ( 'NONE',  ( 57.61547081786810764, 48.90051614449766504, -2.450534656007114176 ) ) ;
#11701 = B_SPLINE_CURVE_WITH_KNOTS ( 'NONE', 3,
 ( #8561, #10827, #124, #12961, #4547, #1343 ),
 .UNSPECIFIED., .F., .F.,
 ( 4, 2, 4 ),
 ( 0.000000000000000000, 0.0002095117440854730670, 0.0004190234881709461339 ),
 .UNSPECIFIED. ) ;
#11702 = LINE ( 'NONE', #2225, #11740 ) ;
#11703 = FACE_OUTER_BOUND ( 'NONE', #5350, .T. ) ;
#11704 = ADVANCED_FACE ( 'NONE', ( #2909, #9344 ), #5208, .T. ) ;
#11705 = CARTESIAN_POINT ( 'NONE',  ( 55.94051828345053679, 59.20051614449766220, 4.345558710429044069 ) ) ;
#11706 =( GEOMETRIC_REPRESENTATION_CONTEXT ( 3 ) GLOBAL_UNCERTAINTY_ASSIGNED_CONTEXT ( ( #6622 ) ) GLOBAL_UNIT_ASSIGNED_CONTEXT ( ( #2494, #10929, #7831 ) ) REPRESENTATION_CONTEXT ( 'NONE', 'WORKASPACE' ) );
#11707 = CARTESIAN_POINT ( 'NONE',  ( 46.49166364869460466, 60.69948385550240033, 4.867452303228209765 ) ) ;
#11708 = AXIS2_PLACEMENT_3D ( 'NONE', #6680, #10878, #1392 ) ;
#11709 = PLANE ( 'NONE',  #3638 ) ;
#11710 = ORIENTED_EDGE ( 'NONE', *, *, #488, .F. ) ;
#11711 = CARTESIAN_POINT ( 'NONE',  ( -62.49999999999997158, 45.00000000000001421, -9.999999999999998224 ) ) ;
#11712 = EDGE_LOOP ( 'NONE', ( #5613, #7683, #10756 ) ) ;
#11713 = CARTESIAN_POINT ( 'NONE',  ( 6.481779955677433591, 2.910222513313285742, 5.040653254389411586 ) ) ;
#11714 = CARTESIAN_POINT ( 'NONE',  ( 0.000000000000000000, 0.000000000000000000, 10.00000000000000000 ) ) ;
#11715 = CARTESIAN_POINT ( 'NONE',  ( 15.00000000000000178, -20.00000000000000000, -50.00000000000000000 ) ) ;
#11716 =( NAMED_UNIT ( * ) SI_UNIT ( $, .STERADIAN. ) SOLID_ANGLE_UNIT ( ) );
#11717 = CARTESIAN_POINT ( 'NONE',  ( 43.34962307344081012, 48.89948385550240317, 2.184720259617164650 ) ) ;
#11718 = AXIS2_PLACEMENT_3D ( 'NONE', #3322, #8714, #11814 ) ;
#11719 = DIRECTION ( 'NONE',  ( 1.000000000000000000, 0.000000000000000000, 0.000000000000000000 ) ) ;
#11720 = CARTESIAN_POINT ( 'NONE',  ( 46.45491332379576477, 51.70051614449765509, 4.840751629271188961 ) ) ;
#11721 = DIRECTION ( 'NONE',  ( 0.000000000000000000, -0.000000000000000000, 1.000000000000000000 ) ) ;
#11722 = CARTESIAN_POINT ( 'NONE',  ( 4.000000000000000000, -2.309401076758516691, -0.4999999999999995559 ) ) ;
#11723 = DIRECTION ( 'NONE',  ( -1.000000000000000000, -0.000000000000000000, 0.000000000000000000 ) ) ;
#11724 = CARTESIAN_POINT ( 'NONE',  ( 43.33558569842703179, 57.09948385550240602, -2.141517661632099223 ) ) ;
#11725 = CARTESIAN_POINT ( 'NONE',  ( 50.02271294988505446, 64.50051614449765225, -7.000000000000000888 ) ) ;
#11726 = EDGE_LOOP ( 'NONE', ( #6017, #5498 ) ) ;
#11727 = VECTOR ( 'NONE', #11783, 1000.000000000000000 ) ;
#11728 = UNCERTAINTY_MEASURE_WITH_UNIT (LENGTH_MEASURE( 1.000000000000000082E-05 ), #5726, 'distance_accuracy_value', 'NONE');
#11729 = EDGE_LOOP ( 'NONE', ( #11604, #8777, #5668, #3013 ) ) ;
#11730 = ORIENTED_EDGE ( 'NONE', *, *, #281, .F. ) ;
#11731 = CARTESIAN_POINT ( 'NONE',  ( 4.104070371397481765, 4.047367226856738220, -5.737475420082528345E-17 ) ) ;
#11732 = LINE ( 'NONE', #6500, #1880 ) ;
#11733 =( BOUNDED_SURFACE ( )  B_SPLINE_SURFACE ( 3, 2, ( 
 ( #10058, #11100, #8966 ),
 ( #7732, #11937, #2456 ),
 ( #12010, #2667, #6695 ),
 ( #1687, #6760, #5867 ),
 ( #10892, #1412, #5727 ),
 ( #9992, #5659, #8000 ) ),
 .UNSPECIFIED., .F., .F., .F. ) 
 B_SPLINE_SURFACE_WITH_KNOTS ( ( 4, 2, 4 ),
 ( 3, 3 ),
 ( 0.02367865728600889244, 0.02663179453327095547, 0.02958493178053301503 ),
 ( 0.000000000000000000, 1.000000000000000000 ),
 .UNSPECIFIED. ) 
 GEOMETRIC_REPRESENTATION_ITEM ( )  RATIONAL_B_SPLINE_SURFACE ( (
 ( 1.000000000000000000, 0.8047781103519378032, 1.000000000000000000),
 ( 1.000000000000000000, 0.8123785825977077879, 1.000000000000000000),
 ( 1.000000000000000000, 0.8190671539292031511, 1.000000000000000000),
 ( 1.000000000000000000, 0.8192352255331103450, 1.000000000000000000),
 ( 1.000000000000000000, 0.8126129676838903526, 1.000000000000000000),
 ( 1.000000000000000000, 0.8047712537969723412, 1.000000000000000000) ) ) 
 REPRESENTATION_ITEM ( '' )  SURFACE ( )  );
#11734 = FACE_OUTER_BOUND ( 'NONE', #13396, .T. ) ;
#11735 = CARTESIAN_POINT ( 'NONE',  ( 0.000000000000000000, 0.000000000000000000, 0.000000000000000000 ) ) ;
#11736 = CARTESIAN_POINT ( 'NONE',  ( 42.63976443033212149, 52.99948385550240459, 0.02388180880522514787 ) ) ;
#11737 = CIRCLE ( 'NONE', #9964, 1.535500000000000087 ) ;
#11738 = CARTESIAN_POINT ( 'NONE',  ( 43.34962307344078880, 48.10051614449766078, -2.184720259617096705 ) ) ;
#11739 = CARTESIAN_POINT ( 'NONE',  ( 0.000000000000000000, 0.000000000000000000, 0.000000000000000000 ) ) ;
#11740 = VECTOR ( 'NONE', #10673, 1000.000000000000000 ) ;
#11741 = CARTESIAN_POINT ( 'NONE',  ( 49.97728705011488159, 47.49948385550240459, -7.000000000000000888 ) ) ;
#11742 = CARTESIAN_POINT ( 'NONE',  ( 0.000000000000000000, 0.000000000000000000, 0.000000000000000000 ) ) ;
#11743 = CARTESIAN_POINT ( 'NONE',  ( 49.97728705011486738, 55.49948385550241170, -8.000000000000001776 ) ) ;
#11744 = EDGE_CURVE ( 'NONE', #13443, #13341, #10134, .T. ) ;
#11745 = VERTEX_POINT ( 'NONE', #7134 ) ;
#11746 = AXIS2_PLACEMENT_3D ( 'NONE', #11621, #11412, #1986 ) ;
#11747 = VERTEX_POINT ( 'NONE', #6377 ) ;
#11748 = VECTOR ( 'NONE', #3070, 1000.000000000000000 ) ;
#11749 = CARTESIAN_POINT ( 'NONE',  ( 2.449293598294706513E-15, -20.00000000000000000, -20.00000000000000000 ) ) ;
#11750 = DIRECTION ( 'NONE',  ( -0.000000000000000000, -0.000000000000000000, 1.000000000000000000 ) ) ;
#11751 = CARTESIAN_POINT ( 'NONE',  ( 56.30877334542961421, 47.00051614449766646, 0.02388180880515774693 ) ) ;
#11752 = CARTESIAN_POINT ( 'NONE',  ( 43.34962307344078880, 62.10051614449766078, -2.184720259617096705 ) ) ;
#11753 = EDGE_CURVE ( 'NONE', #5220, #7288, #7283, .T. ) ;
#11754 = CARTESIAN_POINT ( 'NONE',  ( 52.57664461997811856, 47.59948385550239891, -8.007379884777229506 ) ) ;
#11755 = CARTESIAN_POINT ( 'NONE',  ( 3.948103430090398991, 3.379418997638670596, 1.146674596026254322 ) ) ;
#11756 = EDGE_CURVE ( 'NONE', #7877, #1386, #3080, .T. ) ;
#11757 = CARTESIAN_POINT ( 'NONE',  ( 47.37792948025170858, 55.60051614449765367, 7.992620115222797139 ) ) ;
#11758 = CIRCLE ( 'NONE', #2255, 2.649999999999988365 ) ;
#11759 = ADVANCED_FACE ( 'NONE', ( #7347 ), #10507, .T. ) ;
#11760 = VERTEX_POINT ( 'NONE', #1020 ) ;
#11761 = EDGE_LOOP ( 'NONE', ( #12270, #5458, #13222, #5388 ) ) ;
#11762 = ORIENTED_EDGE ( 'NONE', *, *, #3933, .F. ) ;
#11763 = ORIENTED_EDGE ( 'NONE', *, *, #6379, .F. ) ;
#11764 = CIRCLE ( 'NONE', #8018, 15.00000000000000000 ) ;
#11765 = DIRECTION ( 'NONE',  ( -0.000000000000000000, 1.000000000000000000, -0.000000000000000000 ) ) ;
#11766 = CARTESIAN_POINT ( 'NONE',  ( 53.50000000000000000, 0.000000000000000000, 3.309499999999999886 ) ) ;
#11767 = LINE ( 'NONE', #220, #1562 ) ;
#11768 = SURFACE_SIDE_STYLE ('',( #8867 ) ) ;
#11769 = CIRCLE ( 'NONE', #13524, 9.999999999999998224 ) ;
#11770 = CARTESIAN_POINT ( 'NONE',  ( 55.71335778527780747, 52.09948385550241312, 1.832500667257165983 ) ) ;
#11771 = CARTESIAN_POINT ( 'NONE',  ( 50.00000000000000000, 40.00000000000000000, 0.000000000000000000 ) ) ;
#11772 = CARTESIAN_POINT ( 'NONE',  ( 42.38452918213190657, 47.90051614449765793, 2.450534656007115508 ) ) ;
#11773 = FACE_OUTER_BOUND ( 'NONE', #11074, .T. ) ;
#11774 = CARTESIAN_POINT ( 'NONE',  ( 0.01055556052338981095, 4.575665857285978078, 2.074714256722482997 ) ) ;
#11775 = CARTESIAN_POINT ( 'NONE',  ( 44.05948171654945611, 58.20051614449764799, -4.345558710429044069 ) ) ;
#11776 = CARTESIAN_POINT ( 'NONE',  ( 53.50833635130540955, 59.69948385550240744, -4.867452303228209765 ) ) ;
#11777 = VERTEX_POINT ( 'NONE', #2069 ) ;
#11778 = CARTESIAN_POINT ( 'NONE',  ( 49.97728705011488159, 45.49948385550240459, -7.000000000000000888 ) ) ;
#11779 = ORIENTED_EDGE ( 'NONE', *, *, #505, .F. ) ;
#11780 = DIRECTION ( 'NONE',  ( 0.000000000000000000, 0.000000000000000000, 1.000000000000000000 ) ) ;
#11781 = ADVANCED_BREP_SHAPE_REPRESENTATION ( '', ( #961, #430 ), #13240 ) ;
#11782 = CARTESIAN_POINT ( 'NONE',  ( 1.498123826657877133, -34.92499999999999716, -9.000000000000000000 ) ) ;
#11783 = DIRECTION ( 'NONE',  ( -9.858538378746663627E-23, 5.031452844637890958E-23, -1.000000000000000000 ) ) ;
#11784 = CARTESIAN_POINT ( 'NONE',  ( 44.05948171654949874, 48.79948385550238754, 4.345558710429105354 ) ) ;
#11785 = DIRECTION ( 'NONE',  ( -0.000000000000000000, -0.000000000000000000, 1.000000000000000000 ) ) ;
#11786 = CARTESIAN_POINT ( 'NONE',  ( 46.45491332379576477, 53.70051614449766220, 4.840751629271188961 ) ) ;
#11787 = AXIS2_PLACEMENT_3D ( 'NONE', #7459, #8763, #11662 ) ;
#11788 = DIRECTION ( 'NONE',  ( -1.000000000000000000, 0.000000000000000000, 0.000000000000000000 ) ) ;
#11789 = DIRECTION ( 'NONE',  ( -9.858538378746663627E-23, 5.031452844637890958E-23, -1.000000000000000000 ) ) ;
#11790 = EDGE_CURVE ( 'NONE', #1065, #12805, #12569, .T. ) ;
#11791 = CARTESIAN_POINT ( 'NONE',  ( 6.518095160331716542, -5.866179305615093931, 2.176274696337492837E-17 ) ) ;
#11792 = CARTESIAN_POINT ( 'NONE',  ( 47.70284917648453415, 59.39948385550241028, -6.992620115222774047 ) ) ;
#11793 = LINE ( 'NONE', #2316, #1156 ) ;
#11794 = EDGE_LOOP ( 'NONE', ( #1811, #2822 ) ) ;
#11795 = VECTOR ( 'NONE', #4047, 1000.000000000000000 ) ;
#11796 = VERTEX_POINT ( 'NONE', #2195 ) ;
#11797 = ORIENTED_EDGE ( 'NONE', *, *, #13608, .F. ) ;
#11798 = CARTESIAN_POINT ( 'NONE',  ( -0.5636800770129166693, -4.293361309317430319, -3.531542292955206275 ) ) ;
#11799 = VECTOR ( 'NONE', #2021, 1000.000000000000000 ) ;
#11800 = CYLINDRICAL_SURFACE ( 'NONE', #746, 1.500000000000000666 ) ;
#11801 = CARTESIAN_POINT ( 'NONE',  ( 45.60000000000000142, 0.000000000000000000, 0.000000000000000000 ) ) ;
#11802 = DIRECTION ( 'NONE',  ( -1.000000000000000000, -0.000000000000000000, -0.000000000000000000 ) ) ;
#11803 = CARTESIAN_POINT ( 'NONE',  ( 43.34962307344081012, 52.89948385550240317, 2.184720259617164650 ) ) ;
#11804 = CIRCLE ( 'NONE', #13337, 12.49999999999999645 ) ;
#11805 = CARTESIAN_POINT ( 'NONE',  ( 45.90387839640208512, 56.30051614449765651, -5.676469297603124353 ) ) ;
#11806 = FACE_BOUND ( 'NONE', #7130, .T. ) ;
#11807 = CARTESIAN_POINT ( 'NONE',  ( 42.63976443033212860, 50.99948385550240459, 0.02388180880522514787 ) ) ;
#11808 = DIRECTION ( 'NONE',  ( -0.6520673188974834833, 0.7581610723493047432, 1.805535875966851803E-17 ) ) ;
#11809 = AXIS2_PLACEMENT_3D ( 'NONE', #13246, #13314, #11184 ) ;
#11810 = CARTESIAN_POINT ( 'NONE',  ( 45.27934281921075410, 59.29948385550240886, -6.458785618021043895 ) ) ;
#11811 = VERTEX_POINT ( 'NONE', #4220 ) ;
#11812 = ORIENTED_EDGE ( 'NONE', *, *, #2788, .F. ) ;
#11813 = CARTESIAN_POINT ( 'NONE',  ( -62.49999999999997158, 40.00000000000001421, -9.999999999999998224 ) ) ;
#11814 = DIRECTION ( 'NONE',  ( 0.000000000000000000, 0.000000000000000000, 1.000000000000000000 ) ) ;
#11815 = CARTESIAN_POINT ( 'NONE',  ( 56.30877334542961421, 55.00051614449766646, 0.02388180880515774693 ) ) ;
#11816 = CARTESIAN_POINT ( 'NONE',  ( 52.25172492374528588, 63.40051614449765083, 7.007379884777204637 ) ) ;
#11817 = EDGE_CURVE ( 'NONE', #13042, #5822, #2084, .T. ) ;
#11818 = CARTESIAN_POINT ( 'NONE',  ( 42.38452918213190657, 63.90051614449765793, 2.450534656007115508 ) ) ;
#11819 = CARTESIAN_POINT ( 'NONE',  ( 47.74827507625478518, 56.59948385550238470, 7.007379884777227730 ) ) ;
#11820 = DIRECTION ( 'NONE',  ( -0.000000000000000000, 1.000000000000000000, -0.000000000000000000 ) ) ;
#11821 = B_SPLINE_CURVE_WITH_KNOTS ( 'NONE', 3,
 ( #6267, #971, #10525, #9488, #5223, #11633, #13558, #4168, #5082, #4305, #4034, #9557, #1947, #9426, #5286, #12460 ),
 .UNSPECIFIED., .F., .F.,
 ( 4, 3, 3, 3, 3, 4 ),
 ( 0.000000000000000000, 5.303647860849293065E-05, 0.0001057093501027226378, 0.0001642058037231607288, 0.0002210073443958831293, 0.0002236769549542879461 ),
 .UNSPECIFIED. ) ;
#11822 = CARTESIAN_POINT ( 'NONE',  ( 49.97728705011495265, 57.50051614449766646, 8.000000000000001776 ) ) ;
#11823 = VERTEX_POINT ( 'NONE', #2134 ) ;
#11824 = ORIENTED_EDGE ( 'NONE', *, *, #11405, .F. ) ;
#11825 = ORIENTED_EDGE ( 'NONE', *, *, #5638, .F. ) ;
#11826 = VERTEX_POINT ( 'NONE', #2474 ) ;
#11827 = DIRECTION ( 'NONE',  ( 0.000000000000000000, 0.000000000000000000, -1.000000000000000000 ) ) ;
#11828 = CARTESIAN_POINT ( 'NONE',  ( -29.99999999999999645, -39.99999999999998579, -12.49999999999999822 ) ) ;
#11829 = FILL_AREA_STYLE_COLOUR ( '', #3108 ) ;
#11830 = DIRECTION ( 'NONE',  ( 0.000000000000000000, 0.000000000000000000, 1.000000000000000000 ) ) ;
#11831 = DIRECTION ( 'NONE',  ( 1.000000000000000000, 0.000000000000000000, -0.000000000000000000 ) ) ;
#11832 = CARTESIAN_POINT ( 'NONE',  ( 44.88205777487398507, 55.19948385550240744, -3.688883143319540814 ) ) ;
#11833 = CARTESIAN_POINT ( 'NONE',  ( 54.09612160359792199, 49.30051614449765651, 5.676469297603124353 ) ) ;
#11834 = CARTESIAN_POINT ( 'NONE',  ( 47.37792948025170858, 47.60051614449766078, 7.992620115222797139 ) ) ;
#11835 = APPLICATION_CONTEXT ( 'automotive_design' ) ;
#11836 = CIRCLE ( 'NONE', #6119, 15.00000000000000000 ) ;
#11837 = CARTESIAN_POINT ( 'NONE',  ( -14.92500000000000249, -18.50187617334218970, -9.000000000000000000 ) ) ;
#11838 = CARTESIAN_POINT ( 'NONE',  ( 6.196878017913830305, 5.292377467571572680, -0.8333333333333333703 ) ) ;
#11839 = AXIS2_PLACEMENT_3D ( 'NONE', #9072, #3814, #12245 ) ;
#11840 = CARTESIAN_POINT ( 'NONE',  ( 50.02271294988505446, 56.50051614449766646, -7.000000000000000888 ) ) ;
#11841 = CARTESIAN_POINT ( 'NONE',  ( 55.11794222512601493, 62.19948385550240744, 3.688883143319541702 ) ) ;
#11842 = EDGE_LOOP ( 'NONE', ( #10052, #8080, #12069, #3397 ) ) ;
#11843 = PLANE ( 'NONE',  #9040 ) ;
#11844 = VERTEX_POINT ( 'NONE', #200 ) ;
#11845 = CARTESIAN_POINT ( 'NONE',  ( -14.99999999999999822, -19.99999999999999645, -50.00000000000000000 ) ) ;
#11846 = PRODUCT_DEFINITION_SHAPE ( 'NONE', 'NONE',  #10036 ) ;
#11847 = CARTESIAN_POINT ( 'NONE',  ( 0.000000000000000000, -4.330127018922188320, 2.500000000000010214 ) ) ;
#11848 = CARTESIAN_POINT ( 'NONE',  ( 6.245835795331710294, -1.036512332922514767, 5.105321605219339531 ) ) ;
#11849 = EDGE_CURVE ( 'NONE', #5736, #10124, #7622, .T. ) ;
#11850 = EDGE_CURVE ( 'NONE', #3165, #65, #1914, .T. ) ;
#11851 = SURFACE_SIDE_STYLE ('',( #3423 ) ) ;
#11852 = CARTESIAN_POINT ( 'NONE',  ( 54.09612160359786515, 51.69948385550240744, -5.676469297603166098 ) ) ;
#11853 = EDGE_CURVE ( 'NONE', #8098, #3416, #11131, .T. ) ;
#11854 = CARTESIAN_POINT ( 'NONE',  ( 1.747541505913279281, -3.837784562140273081, -3.503702292528912299 ) ) ;
#11855 = CARTESIAN_POINT ( 'NONE',  ( 55.08986747509849380, 57.20051614449766220, 3.727524721679155384 ) ) ;
#11856 = LINE ( 'NONE', #7785, #1564 ) ;
#11857 = CARTESIAN_POINT ( 'NONE',  ( 62.49999999999998579, 40.00000000000001421, -5.000000000000000000 ) ) ;
#11858 = PRESENTATION_STYLE_ASSIGNMENT (( #10882 ) ) ;
#11859 = CARTESIAN_POINT ( 'NONE',  ( 42.63976443033212860, 60.99948385550238328, 0.02388180880522514787 ) ) ;
#11860 = DIRECTION ( 'NONE',  ( 1.000000000000000000, 0.000000000000000000, 0.000000000000000000 ) ) ;
#11861 = ORIENTED_EDGE ( 'NONE', *, *, #6753, .T. ) ;
#11862 = UNCERTAINTY_MEASURE_WITH_UNIT (LENGTH_MEASURE( 1.000000000000000082E-05 ), #5506, 'distance_accuracy_value', 'NONE');
#11863 = ORIENTED_EDGE ( 'NONE', *, *, #7525, .T. ) ;
#11864 = CARTESIAN_POINT ( 'NONE',  ( -74.99999999999997158, 40.00000000000001421, -10.00000000000000000 ) ) ;
#11865 = DIRECTION ( 'NONE',  ( 0.000000000000000000, 0.000000000000000000, -1.000000000000000000 ) ) ;
#11866 = CARTESIAN_POINT ( 'NONE',  ( 2.000000000000000000, -1.773042676681341856, 2.276824562219559311E-15 ) ) ;
#11867 = DIRECTION ( 'NONE',  ( -0.000000000000000000, -0.000000000000000000, -1.000000000000000000 ) ) ;
#11868 = LINE ( 'NONE', #1215, #13328 ) ;
#11869 = CARTESIAN_POINT ( 'NONE',  ( 44.05948171654949874, 50.79948385550239465, 4.345558710429104465 ) ) ;
#11870 = CARTESIAN_POINT ( 'NONE',  ( 52.25172492374527877, 51.40051614449767214, 7.007379884777203749 ) ) ;
#11871 = FACE_OUTER_BOUND ( 'NONE', #2993, .T. ) ;
#11872 = CARTESIAN_POINT ( 'NONE',  ( 47.70284917648453415, 51.39948385550238896, -6.992620115222774047 ) ) ;
#11873 = B_SPLINE_CURVE_WITH_KNOTS ( 'NONE', 3,
 ( #5231, #7370, #3274, #11579 ),
 .UNSPECIFIED., .F., .F.,
 ( 4, 4 ),
 ( 0.002977824986803813152, 0.005972417098209346735 ),
 .UNSPECIFIED. ) ;
#11874 = DIRECTION ( 'NONE',  ( 0.000000000000000000, 0.000000000000000000, 1.000000000000000000 ) ) ;
#11875 = COLOUR_RGB ( '',1.000000000000000000, 0.9490196078431372140, 0.9098039215686274384 ) ;
#11876 = CARTESIAN_POINT ( 'NONE',  ( 47.37792948025162332, 63.39948385550238896, -7.992620115222770494 ) ) ;
#11877 = ORIENTED_EDGE ( 'NONE', *, *, #1521, .F. ) ;
#11878 = VERTEX_POINT ( 'NONE', #3319 ) ;
#11879 = VERTEX_POINT ( 'NONE', #12775 ) ;
#11880 = CARTESIAN_POINT ( 'NONE',  ( 4.071447262713888016, 4.041451884327382338, 0.000000000000000000 ) ) ;
#11881 = AXIS2_PLACEMENT_3D ( 'NONE', #9872, #391, #8847 ) ;
#11882 = ADVANCED_FACE ( 'NONE', ( #9811 ), #6512, .F. ) ;
#11883 = DIRECTION ( 'NONE',  ( -1.000000000000000000, -0.000000000000000000, -0.000000000000000000 ) ) ;
#11884 = VECTOR ( 'NONE', #5181, 1000.000000000000000 ) ;
#11885 = CARTESIAN_POINT ( 'NONE',  ( 49.97728705011494554, 55.50051614449766646, 6.000000000000000888 ) ) ;
#11886 = CARTESIAN_POINT ( 'NONE',  ( 43.33558569842706021, 63.90051614449765793, 2.141517661632167169 ) ) ;
#11887 = CARTESIAN_POINT ( 'NONE',  ( 50.02271294988513972, 50.49948385550239749, 8.000000000000001776 ) ) ;
#11888 = CARTESIAN_POINT ( 'NONE',  ( 55.94051828345050836, 59.79948385550238754, -4.345558710429104465 ) ) ;
#11889 = CARTESIAN_POINT ( 'NONE',  ( 8.500000000000000000, 0.000000000000000000, 4.000000000000000000 ) ) ;
#11890 = CARTESIAN_POINT ( 'NONE',  ( 43.20883090819745576, 46.79948385550240886, 4.963592699179006473 ) ) ;
#11891 = AXIS2_PLACEMENT_3D ( 'NONE', #6348, #11780, #102 ) ;
#11892 = ORIENTED_EDGE ( 'NONE', *, *, #3183, .T. ) ;
#11893 = AXIS2_PLACEMENT_3D ( 'NONE', #9450, #10416, #13650 ) ;
#11894 = VERTEX_POINT ( 'NONE', #11813 ) ;
#11895 = EDGE_LOOP ( 'NONE', ( #5132, #9455, #669, #10695 ) ) ;
#11896 = VERTEX_POINT ( 'NONE', #8778 ) ;
#11897 = PRODUCT_DEFINITION ( 'UNKNOWN', '', #7729, #4400 ) ;
#11898 = CARTESIAN_POINT ( 'NONE',  ( 2.449293598294706513E-15, -20.00000000000000000, -9.000000000000000000 ) ) ;
#11899 =( LENGTH_UNIT ( ) NAMED_UNIT ( * ) SI_UNIT ( .MILLI., .METRE. ) );
#11900 = CARTESIAN_POINT ( 'NONE',  ( -4.878909776184767981E-16, 0.4887495715076933811, 4.999999999999999112 ) ) ;
#11901 = DIRECTION ( 'NONE',  ( 1.000000000000000000, -0.000000000000000000, -0.000000000000000000 ) ) ;
#11902 = CARTESIAN_POINT ( 'NONE',  ( 49.97728705011488870, 55.49948385550241170, -6.000000000000000888 ) ) ;
#11903 = CARTESIAN_POINT ( 'NONE',  ( 47.70284917648459810, 49.60051614449765367, 6.992620115222797139 ) ) ;
#11904 = CARTESIAN_POINT ( 'NONE',  ( 42.39856655714564226, 50.10051614449766078, -2.493737253992044156 ) ) ;
#11905 = DIRECTION ( 'NONE',  ( 0.000000000000000000, 0.000000000000000000, 1.000000000000000000 ) ) ;
#11906 = CARTESIAN_POINT ( 'NONE',  ( -62.49999999999997158, 20.00000000000001421, 9.999999999999998224 ) ) ;
#11907 = CARTESIAN_POINT ( 'NONE',  ( 43.34962307344078880, 60.10051614449766078, -2.184720259617096705 ) ) ;
#11908 = ORIENTED_EDGE ( 'NONE', *, *, #8193, .F. ) ;
#11909 = AXIS2_PLACEMENT_3D ( 'NONE', #13596, #8432, #9402 ) ;
#11910 = PLANE ( 'NONE',  #7286 ) ;
#11911 = EDGE_CURVE ( 'NONE', #13462, #9655, #6573, .T. ) ;
#11912 = ORIENTED_EDGE ( 'NONE', *, *, #12482, .T. ) ;
#11913 = DIRECTION ( 'NONE',  ( -1.000000000000000000, -0.000000000000000000, -0.000000000000000000 ) ) ;
#11914 = AXIS2_PLACEMENT_3D ( 'NONE', #8947, #9008, #11286 ) ;
#11915 = CARTESIAN_POINT ( 'NONE',  ( -5.686050877451574337, -5.768780236673276995, -1.000000000000000000 ) ) ;
#11916 = CARTESIAN_POINT ( 'NONE',  ( 10.00000000000000000, 25.00000000000001776, 15.00000000000000000 ) ) ;
#11917 = CARTESIAN_POINT ( 'NONE',  ( -62.49999999999997158, 32.50000000000001421, 20.60000000000000142 ) ) ;
#11918 = CARTESIAN_POINT ( 'NONE',  ( 57.36023556966787851, 59.99948385550240459, -0.02388180880522424582 ) ) ;
#11919 = FACE_OUTER_BOUND ( 'NONE', #9507, .T. ) ;
#11920 = CARTESIAN_POINT ( 'NONE',  ( 55.69932041026405045, 61.10051614449766788, 1.875703265242156359 ) ) ;
#11921 = EDGE_CURVE ( 'NONE', #345, #10123, #1159, .T. ) ;
#11922 = DIRECTION ( 'NONE',  ( -0.000000000000000000, -0.000000000000000000, 1.000000000000000000 ) ) ;
#11923 = CARTESIAN_POINT ( 'NONE',  ( -12.17636723815382993, -11.24008670809956456, -9.000000000000000000 ) ) ;
#11924 = CARTESIAN_POINT ( 'NONE',  ( 46.45491332379572924, 47.29948385550241596, -4.840751629271157874 ) ) ;
#11925 = PLANE ( 'NONE',  #100 ) ;
#11926 = EDGE_CURVE ( 'NONE', #347, #12678, #333, .T. ) ;
#11927 = VERTEX_POINT ( 'NONE', #8642 ) ;
#11928 = ORIENTED_EDGE ( 'NONE', *, *, #3563, .T. ) ;
#11929 = EDGE_CURVE ( 'NONE', #5442, #10405, #315, .T. ) ;
#11930 = SHAPE_REPRESENTATION ( 'circlip for shafts normal_din_Circlip DIN 471 - 10 x 1', ( #430 ), #2855 ) ;
#11931 = ORIENTED_EDGE ( 'NONE', *, *, #7218, .T. ) ;
#11932 = FACE_BOUND ( 'NONE', #10421, .T. ) ;
#11933 = MECHANICAL_DESIGN_GEOMETRIC_PRESENTATION_REPRESENTATION (  '', ( #9502 ), #11241 ) ;
#11934 = AXIS2_PLACEMENT_3D ( 'NONE', #1795, #12244, #10306 ) ;
#11935 = CARTESIAN_POINT ( 'NONE',  ( -0.1404048886732797152, -4.699864953788083888, -3.686887068327043160 ) ) ;
#11936 = CARTESIAN_POINT ( 'NONE',  ( 4.175813232069146785, 2.061359961916365613, -3.570380186727397653 ) ) ;
#11937 = CARTESIAN_POINT ( 'NONE',  ( 6.327632967268630004, 3.313549392874629795, 4.260764098153893897 ) ) ;
#11938 = DIRECTION ( 'NONE',  ( 0.000000000000000000, 0.000000000000000000, -1.000000000000000000 ) ) ;
#11939 = CARTESIAN_POINT ( 'NONE',  ( 55.96859303347805081, 54.19948385550240033, 4.306917132069425058 ) ) ;
#11940 = CARTESIAN_POINT ( 'NONE',  ( 55.96859303347802239, 54.80051614449764230, -4.306917132069484566 ) ) ;
#11941 = DIRECTION ( 'NONE',  ( 0.000000000000000000, 0.000000000000000000, -1.000000000000000000 ) ) ;
#11942 = CARTESIAN_POINT ( 'NONE',  ( 45.86712807150323812, 53.29948385550240886, -5.649768623646098220 ) ) ;
#11943 = CARTESIAN_POINT ( 'NONE',  ( 52.29715082351547295, 46.39948385550240317, 6.992620115222774047 ) ) ;
#11944 = VECTOR ( 'NONE', #6482, 1000.000000000000000 ) ;
#11945 = EDGE_CURVE ( 'NONE', #4523, #4643, #13568, .T. ) ;
#11946 = CARTESIAN_POINT ( 'NONE',  ( 52.57664461997811856, 61.59948385550240602, -8.007379884777229506 ) ) ;
#11947 = EDGE_CURVE ( 'NONE', #3673, #8931, #12893, .T. ) ;
#11948 = VERTEX_POINT ( 'NONE', #8574 ) ;
#11949 = ORIENTED_EDGE ( 'NONE', *, *, #5425, .T. ) ;
#11950 = CARTESIAN_POINT ( 'NONE',  ( 0.000000000000000000, 20.00000000000001421, -9.999999999999998224 ) ) ;
#11951 = VERTEX_POINT ( 'NONE', #11677 ) ;
#11952 = DIRECTION ( 'NONE',  ( 0.000000000000000000, 0.000000000000000000, -1.000000000000000000 ) ) ;
#11953 = VECTOR ( 'NONE', #5657, 1000.000000000000227 ) ;
#11954 = PRESENTATION_LAYER_ASSIGNMENT (  '', '', ( #8874 ) ) ;
#11955 = FACE_OUTER_BOUND ( 'NONE', #7941, .T. ) ;
#11956 = CARTESIAN_POINT ( 'NONE',  ( 53.54508667620424234, 54.70051614449765509, -4.840751629271188961 ) ) ;
#11957 = DIRECTION ( 'NONE',  ( -1.000000000000000000, 0.000000000000000000, 0.000000000000000000 ) ) ;
#11958 = CARTESIAN_POINT ( 'NONE',  ( 54.72065718078924590, 54.29948385550241596, 6.458785618021043895 ) ) ;
#11959 = CARTESIAN_POINT ( 'NONE',  ( 52.25172492374522903, 55.59948385550241312, -7.007379884777225953 ) ) ;
#11960 = DIRECTION ( 'NONE',  ( -0.000000000000000000, 1.000000000000000000, -0.000000000000000000 ) ) ;
#11961 = EDGE_CURVE ( 'NONE', #13619, #10697, #2524, .T. ) ;
#11962 = CARTESIAN_POINT ( 'NONE',  ( 58.41169779390614281, 63.00051614449766646, 0.02388180880515032231 ) ) ;
#11963 = AXIS2_PLACEMENT_3D ( 'NONE', #11574, #12794, #7559 ) ;
#11964 = EDGE_CURVE ( 'NONE', #65, #13062, #2200, .T. ) ;
#11965 = PRODUCT_DEFINITION_SHAPE ( 'NONE', 'NONE',  #13675 ) ;
#11966 = AXIS2_PLACEMENT_3D ( 'NONE', #9634, #1959, #7304 ) ;
#11967 = AXIS2_PLACEMENT_3D ( 'NONE', #6823, #10963, #11030 ) ;
#11968 = VERTEX_POINT ( 'NONE', #5535 ) ;
#11969 = ORIENTED_EDGE ( 'NONE', *, *, #11521, .T. ) ;
#11970 = EDGE_LOOP ( 'NONE', ( #6458, #7957, #8011, #13158 ) ) ;
#11971 = ORIENTED_EDGE ( 'NONE', *, *, #3344, .F. ) ;
#11972 = CYLINDRICAL_SURFACE ( 'NONE', #11558, 9.999999999999998224 ) ;
#11973 = B_SPLINE_CURVE_WITH_KNOTS ( 'NONE', 3,
 ( #11105, #1623, #5871, #10064, #4895 ),
 .UNSPECIFIED., .F., .F.,
 ( 4, 1, 4 ),
 ( 5.337851785822274535E-20, 0.002020725942163691374, 0.004041451884327382747 ),
 .UNSPECIFIED. ) ;
#11974 = PLANE ( 'NONE',  #820 ) ;
#11975 = FACE_OUTER_BOUND ( 'NONE', #10314, .T. ) ;
#11976 = CARTESIAN_POINT ( 'NONE',  ( -2.688821387764050996E-14, -4.618802153517012954, -0.4999999999999995559 ) ) ;
#11977 = VECTOR ( 'NONE', #7161, 1000.000000000000000 ) ;
#11978 = CARTESIAN_POINT ( 'NONE',  ( 44.28664221472220675, 57.09948385550240602, -1.832500667257165317 ) ) ;
#11979 = CARTESIAN_POINT ( 'NONE',  ( 43.33558569842706021, 49.90051614449766504, 2.141517661632167169 ) ) ;
#11980 = CARTESIAN_POINT ( 'NONE',  ( 56.81924384183006538, 50.80051614449766362, -4.924951120819380357 ) ) ;
#11981 = CIRCLE ( 'NONE', #4478, 5.000000000000000888 ) ;
#11982 = DIRECTION ( 'NONE',  ( 0.000000000000000000, 0.000000000000000000, 1.000000000000000000 ) ) ;
#11983 = CARTESIAN_POINT ( 'NONE',  ( 51.88965917396063077, 45.00000000000000711, -6.239765512074564313 ) ) ;
#11984 = CARTESIAN_POINT ( 'NONE',  ( 54.68390685589039890, 45.30051614449766362, 6.485486291978072693 ) ) ;
#11985 = ORIENTED_EDGE ( 'NONE', *, *, #9719, .F. ) ;
#11986 = LINE ( 'NONE', #6738, #5075 ) ;
#11987 = ORIENTED_EDGE ( 'NONE', *, *, #12929, .T. ) ;
#11988 = DIRECTION ( 'NONE',  ( -0.000000000000000000, 0.000000000000000000, -1.000000000000000000 ) ) ;
#11989 = AXIS2_PLACEMENT_3D ( 'NONE', #1924, #11404, #11266 ) ;
#11990 = CARTESIAN_POINT ( 'NONE',  ( 13.99999999999999822, 0.000000000000000000, 0.000000000000000000 ) ) ;
#11991 = EDGE_CURVE ( 'NONE', #2116, #582, #1638, .T. ) ;
#11992 = LINE ( 'NONE', #1324, #3556 ) ;
#11993 = DIRECTION ( 'NONE',  ( 0.000000000000000000, 0.000000000000000000, 1.000000000000000000 ) ) ;
#11994 = CARTESIAN_POINT ( 'NONE',  ( 54.09612160359786515, 57.69948385550240744, -5.676469297603166098 ) ) ;
#11995 = CARTESIAN_POINT ( 'NONE',  ( 48.07319477248762496, 58.40051614449765793, -6.007379884777208190 ) ) ;
#11996 = EDGE_CURVE ( 'NONE', #4959, #7826, #68, .T. ) ;
#11997 = FACE_OUTER_BOUND ( 'NONE', #6121, .T. ) ;
#11998 = FACE_OUTER_BOUND ( 'NONE', #9624, .T. ) ;
#11999 = CARTESIAN_POINT ( 'NONE',  ( 55.94051828345053679, 45.20051614449764088, 4.345558710429044069 ) ) ;
#12000 = CARTESIAN_POINT ( 'NONE',  ( 55.69932041026404335, 47.89948385550240317, -1.875703265242203432 ) ) ;
#12001 = DIRECTION ( 'NONE',  ( 1.734723475976806848E-16, 1.000000000000000000, 0.000000000000000000 ) ) ;
#12002 = B_SPLINE_CURVE_WITH_KNOTS ( 'NONE', 3,
 ( #10182, #8878, #422, #688, #9151, #4658, #7845, #2645 ),
 .UNSPECIFIED., .F., .F.,
 ( 4, 2, 2, 4 ),
 ( 0.000000000000000000, 0.002450665683189820997, 0.003675998524784731495, 0.004901331366379641993 ),
 .UNSPECIFIED. ) ;
#12003 = ORIENTED_EDGE ( 'NONE', *, *, #3479, .F. ) ;
#12004 = ORIENTED_EDGE ( 'NONE', *, *, #5437, .T. ) ;
#12005 = ORIENTED_EDGE ( 'NONE', *, *, #12159, .F. ) ;
#12006 = CARTESIAN_POINT ( 'NONE',  ( -20.00000000000000000, -19.99999999999999289, -20.00000000000000000 ) ) ;
#12007 = CARTESIAN_POINT ( 'NONE',  ( 62.49999999999998579, 45.00000000000001421, -15.00000000000000000 ) ) ;
#12008 = DIRECTION ( 'NONE',  ( 1.000000000000000000, 0.000000000000000000, 0.000000000000000000 ) ) ;
#12009 =( NAMED_UNIT ( * ) PLANE_ANGLE_UNIT ( ) SI_UNIT ( $, .RADIAN. ) );
#12010 = CARTESIAN_POINT ( 'NONE',  ( 6.095473853218515536, 3.806361898857873793, 3.407187799183811983 ) ) ;
#12011 = CARTESIAN_POINT ( 'NONE',  ( 4.158413352280813768, -2.044871626972823542, 3.541821552872969736 ) ) ;
#12012 = EDGE_CURVE ( 'NONE', #2436, #7271, #8713, .T. ) ;
#12013 = VECTOR ( 'NONE', #3503, 1000.000000000000000 ) ;
#12014 = CARTESIAN_POINT ( 'NONE',  ( 44.05948171654945611, 54.20051614449764799, -4.345558710429044069 ) ) ;
#12015 = EDGE_CURVE ( 'NONE', #9183, #2907, #10840, .T. ) ;
#12016 = DIRECTION ( 'NONE',  ( -3.469446951953611033E-15, 1.000000000000000000, 0.000000000000000000 ) ) ;
#12017 = CARTESIAN_POINT ( 'NONE',  ( 43.34962307344081012, 54.89948385550240317, 2.184720259617164650 ) ) ;
#12018 = FACE_OUTER_BOUND ( 'NONE', #4402, .T. ) ;
#12019 = CARTESIAN_POINT ( 'NONE',  ( 49.97728705011488159, 45.49948385550240459, -7.000000000000000888 ) ) ;
#12020 = CIRCLE ( 'NONE', #3846, 9.999999999999998224 ) ;
#12021 = VERTEX_POINT ( 'NONE', #3254 ) ;
#12022 = ORIENTED_EDGE ( 'NONE', *, *, #216, .T. ) ;
#12023 = CARTESIAN_POINT ( 'NONE',  ( 20.00000000000000000, -20.00000000000000000, -23.00000000000000000 ) ) ;
#12024 = EDGE_LOOP ( 'NONE', ( #2624, #405 ) ) ;
#12025 = CARTESIAN_POINT ( 'NONE',  ( -74.99999999999998579, 7.499999999999975131, 10.00000000000000000 ) ) ;
#12026 = AXIS2_PLACEMENT_3D ( 'NONE', #7921, #2802, #5921 ) ;
#12027 = AXIS2_PLACEMENT_3D ( 'NONE', #10431, #11468, #3173 ) ;
#12028 = FACE_OUTER_BOUND ( 'NONE', #7878, .T. ) ;
#12029 = EDGE_CURVE ( 'NONE', #5283, #8026, #12152, .T. ) ;
#12030 = CARTESIAN_POINT ( 'NONE',  ( 48.02776887271750184, 53.60051614449765367, 5.992620115222795363 ) ) ;
#12031 = EDGE_CURVE ( 'NONE', #9042, #10299, #1561, .T. ) ;
#12032 = CARTESIAN_POINT ( 'NONE',  ( -2.100000000000000089, 2.571758278209441957E-16, -0.2800830152838844622 ) ) ;
#12033 = CARTESIAN_POINT ( 'NONE',  ( 47.42335538002188144, 50.59948385550240602, 8.007379884777233059 ) ) ;
#12034 = EDGE_CURVE ( 'NONE', #11555, #13173, #4906, .T. ) ;
#12035 = CARTESIAN_POINT ( 'NONE',  ( 44.03140696652192787, 57.19948385550238612, -4.306917132069425058 ) ) ;
#12036 = CYLINDRICAL_SURFACE ( 'NONE', #6048, 2.649999999999988365 ) ;
#12037 = CARTESIAN_POINT ( 'NONE',  ( 57.61547081786810764, 60.90051614449766504, -2.450534656007114176 ) ) ;
#12038 = ORIENTED_EDGE ( 'NONE', *, *, #3170, .T. ) ;
#12039 = CONTEXT_DEPENDENT_SHAPE_REPRESENTATION ( #7082, #6350 ) ;
#12040 = ORIENTED_EDGE ( 'NONE', *, *, #12827, .T. ) ;
#12041 = ORIENTED_EDGE ( 'NONE', *, *, #6895, .F. ) ;
#12042 = VERTEX_POINT ( 'NONE', #1490 ) ;
#12043 = AXIS2_PLACEMENT_3D ( 'NONE', #2875, #12277, #11308 ) ;
#12044 = DIRECTION ( 'NONE',  ( -1.000000000000000000, 0.000000000000000000, 0.000000000000000000 ) ) ;
#12045 = DIRECTION ( 'NONE',  ( 1.000000000000000000, 0.000000000000000000, 0.000000000000000000 ) ) ;
#12046 = CARTESIAN_POINT ( 'NONE',  ( 62.50000000000000000, 20.00000000000001421, 15.00000000000000000 ) ) ;
#12047 = CARTESIAN_POINT ( 'NONE',  ( 48.02776887271745210, 57.39948385550241028, -5.992620115222778487 ) ) ;
#12048 = CARTESIAN_POINT ( 'NONE',  ( 45.90387839640208512, 46.30051614449766362, -5.676469297603124353 ) ) ;
#12049 = CARTESIAN_POINT ( 'NONE',  ( 42.38452918213190657, 49.90051614449766504, 2.450534656007115508 ) ) ;
#12050 = FACE_OUTER_BOUND ( 'NONE', #4119, .T. ) ;
#12051 = CARTESIAN_POINT ( 'NONE',  ( 52.95539523038642926, 45.00000000000002132, -5.827023132204991462 ) ) ;
#12052 = B_SPLINE_CURVE_WITH_KNOTS ( 'NONE', 3,
 ( #11722, #6488, #5110, #13586, #4133, #3494 ),
 .UNSPECIFIED., .F., .F.,
 ( 4, 2, 4 ),
 ( 0.003358874760055551890, 0.004541967308452098118, 0.005725059856848645212 ),
 .UNSPECIFIED. ) ;
#12053 = CARTESIAN_POINT ( 'NONE',  ( 57.61547081786810764, 44.90051614449765793, -2.450534656007114176 ) ) ;
#12054 = VERTEX_POINT ( 'NONE', #10975 ) ;
#12055 = FACE_OUTER_BOUND ( 'NONE', #9687, .T. ) ;
#12056 = ORIENTED_EDGE ( 'NONE', *, *, #3817, .T. ) ;
#12057 = DIRECTION ( 'NONE',  ( 0.000000000000000000, 0.000000000000000000, 1.000000000000000000 ) ) ;
#12058 = CARTESIAN_POINT ( 'NONE',  ( 4.175813232069148562, 4.122719923832741884, -2.765695189283172261E-17 ) ) ;
#12059 = CIRCLE ( 'NONE', #11399, 2.500000000000000444 ) ;
#12060 = DIRECTION ( 'NONE',  ( 0.000000000000000000, 0.000000000000000000, -1.000000000000000000 ) ) ;
#12061 = CARTESIAN_POINT ( 'NONE',  ( 55.96859303347804371, 60.19948385550240744, 4.306917132069425946 ) ) ;
#12062 = ADVANCED_FACE ( 'NONE', ( #4631, #7946 ), #6908, .F. ) ;
#12063 = CARTESIAN_POINT ( 'NONE',  ( 51.97223112728249816, 60.60051614449765367, -5.992620115222793586 ) ) ;
#12064 = LINE ( 'NONE', #8059, #2335 ) ;
#12065 = CARTESIAN_POINT ( 'NONE',  ( 3.679171394226031122, 2.494631558665830973, -0.3503314178412474389 ) ) ;
#12066 = CARTESIAN_POINT ( 'NONE',  ( 54.09612160359792199, 45.30051614449766362, 5.676469297603124353 ) ) ;
#12067 = CARTESIAN_POINT ( 'NONE',  ( 46.49166364869460466, 48.69948385550241454, 4.867452303228209765 ) ) ;
#12068 = DIRECTION ( 'NONE',  ( 1.000000000000000000, 0.000000000000000000, 0.000000000000000000 ) ) ;
#12069 = ORIENTED_EDGE ( 'NONE', *, *, #6140, .T. ) ;
#12070 = EDGE_CURVE ( 'NONE', #6246, #2319, #8979, .T. ) ;
#12071 = ORIENTED_EDGE ( 'NONE', *, *, #1404, .F. ) ;
#12072 = DIRECTION ( 'NONE',  ( -1.000000000000000000, 0.000000000000000000, -0.000000000000000000 ) ) ;
#12073 = PRODUCT_DEFINITION ( 'UNKNOWN', '', #12359, #6885 ) ;
#12074 = CARTESIAN_POINT ( 'NONE',  ( 0.5276280594147412240, -4.314175951381924889, -3.320322319201654881 ) ) ;
#12075 = DIRECTION ( 'NONE',  ( -0.8191520442889875797, 1.003171929053519570E-16, 0.5735764363510522656 ) ) ;
#12076 = FACE_OUTER_BOUND ( 'NONE', #7825, .T. ) ;
#12077 = DIRECTION ( 'NONE',  ( 0.000000000000000000, 0.000000000000000000, -1.000000000000000000 ) ) ;
#12078 = CARTESIAN_POINT ( 'NONE',  ( 52.29715082351538769, 62.60051614449766078, -6.992620115222796251 ) ) ;
#12079 = CARTESIAN_POINT ( 'NONE',  ( 6.323268674613562013, -2.010012106699304191, -5.000000000001305622 ) ) ;
#12080 = DIRECTION ( 'NONE',  ( 0.000000000000000000, -0.5000000000000011102, -0.8660254037844379305 ) ) ;
#12081 = CARTESIAN_POINT ( 'NONE',  ( 54.13287192849676188, 50.29948385550240175, 5.649768623646098220 ) ) ;
#12082 = CARTESIAN_POINT ( 'NONE',  ( 56.66441430157296821, 48.09948385550240602, 2.141517661632100111 ) ) ;
#12083 = CARTESIAN_POINT ( 'NONE',  ( 54.72065718078924590, 60.29948385550240175, 6.458785618021043895 ) ) ;
#12084 = ORIENTED_EDGE ( 'NONE', *, *, #5017, .F. ) ;
#12085 = EDGE_LOOP ( 'NONE', ( #3096, #10219, #2132 ) ) ;
#12086 = LINE ( 'NONE', #5876, #10103 ) ;
#12087 = ORIENTED_EDGE ( 'NONE', *, *, #9007, .T. ) ;
#12088 = CARTESIAN_POINT ( 'NONE',  ( 6.271006797790669829, -0.9853839345309097775, -5.106080050406711202 ) ) ;
#12089 = EDGE_CURVE ( 'NONE', #3673, #7167, #655, .T. ) ;
#12090 = CARTESIAN_POINT ( 'NONE',  ( 6.495567275915079541, -2.917443832164891226, -5.053160945538031967 ) ) ;
#12091 = CARTESIAN_POINT ( 'NONE',  ( 50.02271294988506156, 56.50051614449767357, -6.000000000000000888 ) ) ;
#12092 = CARTESIAN_POINT ( 'NONE',  ( 54.09612160359792199, 63.30051614449766362, 5.676469297603124353 ) ) ;
#12093 = CARTESIAN_POINT ( 'NONE',  ( 45.31609314410967926, 50.69948385550240744, 6.485486291978119766 ) ) ;
#12094 = CARTESIAN_POINT ( 'NONE',  ( 45.86712807150323812, 55.29948385550240175, -5.649768623646098220 ) ) ;
#12095 = DIRECTION ( 'NONE',  ( -0.000000000000000000, -0.000000000000000000, 1.000000000000000000 ) ) ;
#12096 = ADVANCED_FACE ( 'NONE', ( #9048 ), #8919, .F. ) ;
#12097 = CARTESIAN_POINT ( 'NONE',  ( 54.68390685589033495, 45.69948385550240033, -6.485486291978119766 ) ) ;
#12098 = ORIENTED_EDGE ( 'NONE', *, *, #12758, .T. ) ;
#12099 = EDGE_CURVE ( 'NONE', #8346, #7656, #5723, .T. ) ;
#12100 = CONTEXT_DEPENDENT_SHAPE_REPRESENTATION ( #1860, #145 ) ;
#12101 = ORIENTED_EDGE ( 'NONE', *, *, #13109, .T. ) ;
#12102 = EDGE_CURVE ( 'NONE', #13025, #5152, #12294, .T. ) ;
#12103 = ORIENTED_EDGE ( 'NONE', *, *, #11649, .T. ) ;
#12104 = AXIS2_PLACEMENT_3D ( 'NONE', #13133, #3675, #7897 ) ;
#12105 = ORIENTED_EDGE ( 'NONE', *, *, #4935, .F. ) ;
#12106 = DIRECTION ( 'NONE',  ( -0.000000000000000000, 1.000000000000000000, -0.000000000000000000 ) ) ;
#12107 = SURFACE_STYLE_FILL_AREA ( #7898 ) ;
#12108 = CARTESIAN_POINT ( 'NONE',  ( -12.99038105676659427, -12.50000000000003020, -9.000000000000000000 ) ) ;
#12109 = EDGE_CURVE ( 'NONE', #345, #13190, #529, .T. ) ;
#12110 = CARTESIAN_POINT ( 'NONE',  ( -4.997494388800372001E-16, -0.4883827417527024095, 4.999999999999999112 ) ) ;
#12111 = CARTESIAN_POINT ( 'NONE',  ( 46.45491332379572924, 57.29948385550240175, -4.840751629271157874 ) ) ;
#12112 = CARTESIAN_POINT ( 'NONE',  ( 56.65037692655921120, 45.10051614449766078, 2.184720259617097593 ) ) ;
#12113 = CARTESIAN_POINT ( 'NONE',  ( 45.27934281921082516, 49.70051614449766220, 6.458785618021089192 ) ) ;
#12114 = DIRECTION ( 'NONE',  ( 1.000000000000000000, 0.000000000000000000, 0.000000000000000000 ) ) ;
#12115 = CARTESIAN_POINT ( 'NONE',  ( 53.45216259278994642, 45.00000000000002132, -5.549029329376620190 ) ) ;
#12116 = CARTESIAN_POINT ( 'NONE',  ( 52.25172492374527877, 61.40051614449765083, 7.007379884777203749 ) ) ;
#12117 =( GEOMETRIC_REPRESENTATION_CONTEXT ( 3 ) GLOBAL_UNCERTAINTY_ASSIGNED_CONTEXT ( ( #5153 ) ) GLOBAL_UNIT_ASSIGNED_CONTEXT ( ( #4129, #3913, #9313 ) ) REPRESENTATION_CONTEXT ( 'NONE', 'WORKASPACE' ) );
#12118 = ORIENTED_EDGE ( 'NONE', *, *, #2465, .T. ) ;
#12119 = DIRECTION ( 'NONE',  ( 1.000000000000000000, -1.734723475976807341E-16, -0.000000000000000000 ) ) ;
#12120 = ORIENTED_EDGE ( 'NONE', *, *, #4584, .T. ) ;
#12121 = CIRCLE ( 'NONE', #5730, 1.999999999999998224 ) ;
#12122 = DIRECTION ( 'NONE',  ( 0.000000000000000000, 0.000000000000000000, -1.000000000000000000 ) ) ;
#12123 = DIRECTION ( 'NONE',  ( -1.000000000000000000, 0.000000000000000000, 0.000000000000000000 ) ) ;
#12124 = DIRECTION ( 'NONE',  ( -1.000000000000000000, 0.000000000000000000, 6.123233995736766036E-17 ) ) ;
#12125 = CARTESIAN_POINT ( 'NONE',  ( 54.13287192849676188, 56.29948385550240175, 5.649768623646098220 ) ) ;
#12126 = AXIS2_PLACEMENT_3D ( 'NONE', #294, #4449, #12871 ) ;
#12127 = CARTESIAN_POINT ( 'NONE',  ( 44.28664221472221385, 55.90051614449766504, 1.832500667257213722 ) ) ;
#12128 = CARTESIAN_POINT ( 'NONE',  ( 3.972709601346593455, -3.429395227388317036, -1.191688283765307110 ) ) ;
#12129 = MECHANICAL_DESIGN_GEOMETRIC_PRESENTATION_REPRESENTATION (  '', ( #8819 ), #5302 ) ;
#12130 = FACE_BOUND ( 'NONE', #13607, .T. ) ;
#12131 = CARTESIAN_POINT ( 'NONE',  ( 57.36023556966787851, 45.00051614449763804, 0.02388180880515038476 ) ) ;
#12132 = CARTESIAN_POINT ( 'NONE',  ( 50.02271294988512551, 64.49948385550240459, 7.000000000000000888 ) ) ;
#12133 = AXIS2_PLACEMENT_3D ( 'NONE', #6838, #463, #4910 ) ;
#12134 = PLANE ( 'NONE',  #4969 ) ;
#12135 = ORIENTED_EDGE ( 'NONE', *, *, #9145, .F. ) ;
#12136 = EDGE_CURVE ( 'NONE', #10104, #9655, #9988, .T. ) ;
#12137 = PRODUCT_DEFINITION_CONTEXT ( 'detailed design', #6389, 'design' ) ;
#12138 = ORIENTED_EDGE ( 'NONE', *, *, #7118, .T. ) ;
#12139 = DIRECTION ( 'NONE',  ( 0.000000000000000000, 0.000000000000000000, -1.000000000000000000 ) ) ;
#12140 = CARTESIAN_POINT ( 'NONE',  ( 1.257172072275274388, -3.892973519170983110, -3.433252694550781303 ) ) ;
#12141 = AXIS2_PLACEMENT_3D ( 'NONE', #6943, #4800, #11011 ) ;
#12142 = CARTESIAN_POINT ( 'NONE',  ( -74.99999999999997158, -39.99999999999998579, 10.00000000000000000 ) ) ;
#12143 = CIRCLE ( 'NONE', #12792, 1.500000000000001332 ) ;
#12144 = DIRECTION ( 'NONE',  ( -1.000000000000000000, -0.000000000000000000, -0.000000000000000000 ) ) ;
#12145 = DIRECTION ( 'NONE',  ( 1.000000000000000000, 0.000000000000000000, 0.000000000000000000 ) ) ;
#12146 = CARTESIAN_POINT ( 'NONE',  ( 45.90387839640208512, 58.30051614449766362, -5.676469297603124353 ) ) ;
#12147 = DIRECTION ( 'NONE',  ( -0.000000000000000000, 1.000000000000000000, -0.000000000000000000 ) ) ;
#12148 = CARTESIAN_POINT ( 'NONE',  ( 4.000000000000000000, -2.309401076758516691, -0.4999999999999995559 ) ) ;
#12149 = CARTESIAN_POINT ( 'NONE',  ( 55.96859303347804371, 56.19948385550241454, 4.306917132069425946 ) ) ;
#12150 =( NAMED_UNIT ( * ) SI_UNIT ( $, .STERADIAN. ) SOLID_ANGLE_UNIT ( ) );
#12151 = CARTESIAN_POINT ( 'NONE',  ( 57.60143344285433642, 63.89948385550240317, -2.493737253992118319 ) ) ;
#12152 = B_SPLINE_CURVE_WITH_KNOTS ( 'NONE', 3,
 ( #7473, #8014, #11043, #393, #5878, #9874 ),
 .UNSPECIFIED., .F., .F.,
 ( 4, 2, 4 ),
 ( 0.003805861006858101119, 0.004828937052660003254, 0.005852013098461904955 ),
 .UNSPECIFIED. ) ;
#12153 = VECTOR ( 'NONE', #13612, 1000.000000000000000 ) ;
#12154 = VERTEX_POINT ( 'NONE', #13045 ) ;
#12155 = ORIENTED_EDGE ( 'NONE', *, *, #5857, .T. ) ;
#12156 = DIRECTION ( 'NONE',  ( -1.000000000000000000, 0.000000000000000000, 0.000000000000000000 ) ) ;
#12157 = VERTEX_POINT ( 'NONE', #583 ) ;
#12158 = DIRECTION ( 'NONE',  ( 1.000000000000000000, 3.469446951953615175E-16, 0.000000000000000000 ) ) ;
#12159 = EDGE_CURVE ( 'NONE', #3838, #6230, #4304, .T. ) ;
#12160 = CARTESIAN_POINT ( 'NONE',  ( 6.420058897733093239, -2.891482565094600776, -5.008194711943422917 ) ) ;
#12161 = CARTESIAN_POINT ( 'NONE',  ( 53.50833635130544508, 63.30051614449767072, 4.867452303228181343 ) ) ;
#12162 = AXIS2_PLACEMENT_3D ( 'NONE', #11612, #1151, #11472 ) ;
#12163 = DIRECTION ( 'NONE',  ( 1.000000000000000000, 3.469446951953615668E-16, -0.000000000000000000 ) ) ;
#12164 = CARTESIAN_POINT ( 'NONE',  ( 47.42335538002188144, 52.59948385550240602, 8.007379884777233059 ) ) ;
#12165 = CARTESIAN_POINT ( 'NONE',  ( 42.63976443033212860, 64.99948385550240459, 0.02388180880522514787 ) ) ;
#12166 = DIRECTION ( 'NONE',  ( -0.000000000000000000, -0.000000000000000000, -1.000000000000000000 ) ) ;
#12167 = ADVANCED_FACE ( 'NONE', ( #3790 ), #11370, .T. ) ;
#12168 = CARTESIAN_POINT ( 'NONE',  ( 47.37792948025170858, 63.60051614449764656, 7.992620115222797139 ) ) ;
#12169 = ORIENTED_EDGE ( 'NONE', *, *, #7136, .T. ) ;
#12170 = VERTEX_POINT ( 'NONE', #1704 ) ;
#12171 = ORIENTED_EDGE ( 'NONE', *, *, #7727, .T. ) ;
#12172 = VERTEX_POINT ( 'NONE', #524 ) ;
#12173 = LINE ( 'NONE', #5758, #1484 ) ;
#12174 = EDGE_CURVE ( 'NONE', #1912, #7290, #4080, .T. ) ;
#12175 = CARTESIAN_POINT ( 'NONE',  ( 75.00000000000000000, 32.50000000000001421, 15.00000000000000000 ) ) ;
#12176 = CARTESIAN_POINT ( 'NONE',  ( 8.500000000000000000, 4.898587196589412829E-16, -4.000000000000000000 ) ) ;
#12177 =( NAMED_UNIT ( * ) SI_UNIT ( $, .STERADIAN. ) SOLID_ANGLE_UNIT ( ) );
#12178 = CARTESIAN_POINT ( 'NONE',  ( 48.02776887271745210, 63.39948385550238896, -5.992620115222778487 ) ) ;
#12179 = CARTESIAN_POINT ( 'NONE',  ( 45.90387839640208512, 50.30051614449766362, -5.676469297603124353 ) ) ;
#12180 = ADVANCED_FACE ( 'NONE', ( #3861 ), #3415, .T. ) ;
#12181 = CARTESIAN_POINT ( 'NONE',  ( 54.68390685589039890, 53.30051614449767072, 6.485486291978072693 ) ) ;
#12182 = CIRCLE ( 'NONE', #11963, 2.100000000000000089 ) ;
#12183 = ADVANCED_FACE ( 'NONE', ( #4207 ), #7193, .T. ) ;
#12184 = CARTESIAN_POINT ( 'NONE',  ( 0.2182387239031248760, 1.693823289467350168, 3.500000000000000000 ) ) ;
#12185 =( GEOMETRIC_REPRESENTATION_CONTEXT ( 3 ) GLOBAL_UNCERTAINTY_ASSIGNED_CONTEXT ( ( #12457 ) ) GLOBAL_UNIT_ASSIGNED_CONTEXT ( ( #1588, #10503, #11551 ) ) REPRESENTATION_CONTEXT ( 'NONE', 'WORKASPACE' ) );
#12186 = CARTESIAN_POINT ( 'NONE',  ( 2.000000000000000000, 1.880445160090761061E-16, -1.535500000000000087 ) ) ;
#12187 = CIRCLE ( 'NONE', #6024, 3.299999999999999822 ) ;
#12188 = CARTESIAN_POINT ( 'NONE',  ( 42.39856655714564226, 46.10051614449766078, -2.493737253992044156 ) ) ;
#12189 = ORIENTED_EDGE ( 'NONE', *, *, #11756, .T. ) ;
#12190 = CARTESIAN_POINT ( 'NONE',  ( 2.000000000000008882, 3.464101615137749945, 0.000000000000000000 ) ) ;
#12191 = ORIENTED_EDGE ( 'NONE', *, *, #12581, .F. ) ;
#12192 = DIRECTION ( 'NONE',  ( -1.224646799147353207E-16, 0.000000000000000000, -1.000000000000000000 ) ) ;
#12193 = DIRECTION ( 'NONE',  ( 1.000000000000000000, 0.000000000000000000, -0.000000000000000000 ) ) ;
#12194 = CARTESIAN_POINT ( 'NONE',  ( 43.33558569842703179, 59.09948385550240602, -2.141517661632099223 ) ) ;
#12195 = CARTESIAN_POINT ( 'NONE',  ( 52.25172492374522903, 61.59948385550239891, -7.007379884777227730 ) ) ;
#12196 = DIRECTION ( 'NONE',  ( 1.000000000000000000, 0.000000000000000000, 0.000000000000000000 ) ) ;
#12197 = CARTESIAN_POINT ( 'NONE',  ( 2.000000000000000000, -1.773042676681341856, 2.276824562219559311E-15 ) ) ;
#12198 = DIRECTION ( 'NONE',  ( -1.000000000000000000, 0.000000000000000000, 0.000000000000000000 ) ) ;
#12199 = CARTESIAN_POINT ( 'NONE',  ( 52.25172492374527877, 47.40051614449766504, 7.007379884777203749 ) ) ;
#12200 = CARTESIAN_POINT ( 'NONE',  ( 55.69932041026404335, 53.89948385550240317, -1.875703265242203432 ) ) ;
#12201 = FACE_OUTER_BOUND ( 'NONE', #2678, .T. ) ;
#12202 = VERTEX_POINT ( 'NONE', #12427 ) ;
#12203 = CONICAL_SURFACE ( 'NONE', #13514, 4.000000000000000000, 0.8911886515913786111 ) ;
#12204 = ORIENTED_EDGE ( 'NONE', *, *, #12241, .T. ) ;
#12205 = ORIENTED_EDGE ( 'NONE', *, *, #9016, .T. ) ;
#12206 = DIRECTION ( 'NONE',  ( -1.000000000000000000, 0.000000000000000000, 0.000000000000000000 ) ) ;
#12207 = VECTOR ( 'NONE', #215, 1000.000000000000000 ) ;
#12208 = CARTESIAN_POINT ( 'NONE',  ( 5.000000000000003553, -20.00000000000000000, -8.999999999999998224 ) ) ;
#12209 = CARTESIAN_POINT ( 'NONE',  ( -1.250000000000000000, -6.429618962271402616, -1.000000000000000000 ) ) ;
#12210 = FACE_OUTER_BOUND ( 'NONE', #4607, .T. ) ;
#12211 = CARTESIAN_POINT ( 'NONE',  ( 4.104070371397484429, -2.023683613428364669, 3.505122836902509587 ) ) ;
#12212 = EDGE_CURVE ( 'NONE', #1302, #8472, #6312, .T. ) ;
#12213 = CARTESIAN_POINT ( 'NONE',  ( 55.96859303347802239, 60.80051614449764941, -4.306917132069484566 ) ) ;
#12214 = DIRECTION ( 'NONE',  ( 0.000000000000000000, 0.000000000000000000, 1.000000000000000000 ) ) ;
#12215 = CARTESIAN_POINT ( 'NONE',  ( 49.97728705011488870, 65.49948385550240459, -6.000000000000000888 ) ) ;
#12216 = CARTESIAN_POINT ( 'NONE',  ( 1.925929944387235853E-31, 15.00000000000001599, 15.00000000000000000 ) ) ;
#12217 = CARTESIAN_POINT ( 'NONE',  ( 43.33558569842703179, 61.09948385550240602, -2.141517661632099223 ) ) ;
#12218 = CARTESIAN_POINT ( 'NONE',  ( 43.33558569842703179, 47.09948385550240602, -2.141517661632099223 ) ) ;
#12219 = CARTESIAN_POINT ( 'NONE',  ( 43.34962307344081012, 46.89948385550240317, 2.184720259617164650 ) ) ;
#12220 = ORIENTED_EDGE ( 'NONE', *, *, #9731, .T. ) ;
#12221 = ORIENTED_EDGE ( 'NONE', *, *, #2638, .F. ) ;
#12222 = FACE_OUTER_BOUND ( 'NONE', #634, .T. ) ;
#12223 = VERTEX_POINT ( 'NONE', #11323 ) ;
#12224 = CARTESIAN_POINT ( 'NONE',  ( 0.000000000000000000, 3.031088913245533423, -1.750000000000004885 ) ) ;
#12225 = CARTESIAN_POINT ( 'NONE',  ( 6.506987859255520590, -2.925375531177299759, -5.066899051217866656 ) ) ;
#12226 = CARTESIAN_POINT ( 'NONE',  ( 55.11794222512599362, 62.80051614449766362, -3.688883143319583446 ) ) ;
#12227 = FACE_OUTER_BOUND ( 'NONE', #10738, .T. ) ;
#12228 = CARTESIAN_POINT ( 'NONE',  ( 52.57664461997811856, 59.59948385550240602, -8.007379884777229506 ) ) ;
#12229 = CARTESIAN_POINT ( 'NONE',  ( 47.70284917648453415, 65.39948385550239607, -6.992620115222774047 ) ) ;
#12230 = CARTESIAN_POINT ( 'NONE',  ( -4.000000000000004441, 2.309401076758496263, -3.504269196027523847 ) ) ;
#12231 = AXIS2_PLACEMENT_3D ( 'NONE', #1530, #10185, #4036 ) ;
#12232 = CARTESIAN_POINT ( 'NONE',  ( 56.79116909180255135, 49.79948385550240175, -4.963592699179005585 ) ) ;
#12233 = ORIENTED_EDGE ( 'NONE', *, *, #6966, .T. ) ;
#12234 = VERTEX_POINT ( 'NONE', #869 ) ;
#12235 = ORIENTED_EDGE ( 'NONE', *, *, #2109, .T. ) ;
#12236 = EDGE_CURVE ( 'NONE', #407, #13146, #11143, .T. ) ;
#12237 = ORIENTED_EDGE ( 'NONE', *, *, #12761, .F. ) ;
#12238 = CIRCLE ( 'NONE', #7841, 1.535500000000000087 ) ;
#12239 = CARTESIAN_POINT ( 'NONE',  ( 0.1739375980333479343, -3.358985280702903253, -4.182066831946573693 ) ) ;
#12240 = FACE_OUTER_BOUND ( 'NONE', #6939, .T. ) ;
#12241 = EDGE_CURVE ( 'NONE', #3165, #11058, #432, .T. ) ;
#12242 = VECTOR ( 'NONE', #9527, 1000.000000000000114 ) ;
#12243 = CARTESIAN_POINT ( 'NONE',  ( -0.9999999999999995559, -15.10102051443364246, -8.999999999999998224 ) ) ;
#12244 = DIRECTION ( 'NONE',  ( 0.9989677110047502362, 0.04542589977017699732, -6.931730960091013400E-15 ) ) ;
#12245 = DIRECTION ( 'NONE',  ( 0.000000000000000000, 0.000000000000000000, 1.000000000000000000 ) ) ;
#12246 = CARTESIAN_POINT ( 'NONE',  ( 43.69122665457040000, 62.99948385550241170, 0.02388180880521036456 ) ) ;
#12247 = CARTESIAN_POINT ( 'NONE',  ( 52.25172492374528588, 55.40051614449765083, 7.007379884777204637 ) ) ;
#12248 = VECTOR ( 'NONE', #12080, 1000.000000000000114 ) ;
#12249 = CARTESIAN_POINT ( 'NONE',  ( 47.42335538002180328, 62.40051614449765793, -8.007379884777206414 ) ) ;
#12250 = CARTESIAN_POINT ( 'NONE',  ( 4.200000000000001954, 0.000000000000000000, 0.000000000000000000 ) ) ;
#12251 = DIRECTION ( 'NONE',  ( -0.7779254092217071648, -0.6283566325640553840, 0.000000000000000000 ) ) ;
#12252 = CARTESIAN_POINT ( 'NONE',  ( 45.31609314410960820, 50.30051614449766362, -6.485486291978072693 ) ) ;
#12253 = VECTOR ( 'NONE', #249, 1000.000000000000000 ) ;
#12255 = EDGE_LOOP ( 'NONE', ( #4711, #13539, #10181, #1098 ) ) ;
#12254 = ORIENTED_EDGE ( 'NONE', *, *, #13406, .F. ) ;
#12256 = CARTESIAN_POINT ( 'NONE',  ( -2.000000000000007550, -3.464101615137749945, 0.000000000000000000 ) ) ;
#12257 = EDGE_LOOP ( 'NONE', ( #5789, #7725, #2402, #2871 ) ) ;
#12258 = CARTESIAN_POINT ( 'NONE',  ( 20.00000000000000000, -25.00000000000000711, -20.00000000000000000 ) ) ;
#12259 = CYLINDRICAL_SURFACE ( 'NONE', #904, 1.500000000000001332 ) ;
#12260 = APPLICATION_PROTOCOL_DEFINITION ( 'draft international standard', 'automotive_design', 1998, #5938 ) ;
#12261 = CARTESIAN_POINT ( 'NONE',  ( 54.13287192849676188, 62.29948385550240886, 5.649768623646098220 ) ) ;
#12262 = CARTESIAN_POINT ( 'NONE',  ( 47.70284917648453415, 57.39948385550240317, -6.992620115222774047 ) ) ;
#12263 = EDGE_CURVE ( 'NONE', #12042, #9288, #8538, .T. ) ;
#12264 = DIRECTION ( 'NONE',  ( -0.000000000000000000, 1.000000000000000000, 1.224646799147353207E-16 ) ) ;
#12265 = CARTESIAN_POINT ( 'NONE',  ( 0.000000000000000000, 0.000000000000000000, -1.000000000000000000 ) ) ;
#12266 = DIRECTION ( 'NONE',  ( 0.000000000000000000, 0.000000000000000000, -1.000000000000000000 ) ) ;
#12267 = CARTESIAN_POINT ( 'NONE',  ( 45.90387839640208512, 46.30051614449766362, -5.676469297603124353 ) ) ;
#12268 = CARTESIAN_POINT ( 'NONE',  ( 53.54508667620428497, 50.29948385550240886, 4.840751629271157874 ) ) ;
#12269 = CARTESIAN_POINT ( 'NONE',  ( 20.00000000000000000, -20.00000000000000000, -20.00000000000000000 ) ) ;
#12270 = ORIENTED_EDGE ( 'NONE', *, *, #12929, .F. ) ;
#12271 = ORIENTED_EDGE ( 'NONE', *, *, #8387, .F. ) ;
#12273 = EDGE_CURVE ( 'NONE', #3939, #13041, #13331, .T. ) ;
#12272 = ORIENTED_EDGE ( 'NONE', *, *, #2122, .T. ) ;
#12274 = CARTESIAN_POINT ( 'NONE',  ( 4.175075985190096262, -2.060370777630117889, -3.568666869285569643 ) ) ;
#12275 = EDGE_CURVE ( 'NONE', #1384, #11826, #4748, .T. ) ;
#12276 = AXIS2_PLACEMENT_3D ( 'NONE', #10610, #8274, #11520 ) ;
#12277 = DIRECTION ( 'NONE',  ( -0.000000000000000000, -0.000000000000000000, -1.000000000000000000 ) ) ;
#12278 = CYLINDRICAL_SURFACE ( 'NONE', #9953, 2.500000000000000444 ) ;
#12279 = FACE_OUTER_BOUND ( 'NONE', #1422, .T. ) ;
#12280 = SURFACE_SIDE_STYLE ('',( #10666 ) ) ;
#12281 = FACE_OUTER_BOUND ( 'NONE', #8946, .T. ) ;
#12282 = CARTESIAN_POINT ( 'NONE',  ( 55.71335778527780747, 64.09948385550239891, 1.832500667257165983 ) ) ;
#12283 = CARTESIAN_POINT ( 'NONE',  ( 4.688877333453707941, -18.97314589549297281, 9.999999999999998224 ) ) ;
#12284 = CARTESIAN_POINT ( 'NONE',  ( 56.66441430157296821, 56.09948385550240602, 2.141517661632100111 ) ) ;
#12285 = CARTESIAN_POINT ( 'NONE',  ( 55.94051828345050836, 53.79948385550238754, -4.345558710429104465 ) ) ;
#12286 = APPLICATION_CONTEXT ( 'automotive_design' ) ;
#12287 = EDGE_LOOP ( 'NONE', ( #6887, #8219 ) ) ;
#12288 = CARTESIAN_POINT ( 'NONE',  ( 52.29715082351547295, 46.39948385550240317, 6.992620115222774047 ) ) ;
#12289 = ORIENTED_EDGE ( 'NONE', *, *, #12015, .F. ) ;
#12290 = ORIENTED_EDGE ( 'NONE', *, *, #11756, .F. ) ;
#12291 = CARTESIAN_POINT ( 'NONE',  ( 3.950250160040163383, -0.7258013381021514165, 3.499999999999845013 ) ) ;
#12292 = EDGE_CURVE ( 'NONE', #2771, #13537, #13122, .T. ) ;
#12293 = VERTEX_POINT ( 'NONE', #4140 ) ;
#12294 = LINE ( 'NONE', #460, #970 ) ;
#12295 = CARTESIAN_POINT ( 'NONE',  ( 6.452281807715810835, -2.898928808472999830, -5.021091983800332947 ) ) ;
#12296 = CARTESIAN_POINT ( 'NONE',  ( 44.88205777487401349, 61.80051614449766362, 3.688883143319584779 ) ) ;
#12297 = CARTESIAN_POINT ( 'NONE',  ( 4.000000000000000000, 2.512223110932545023, -3.469391141908803711 ) ) ;
#12298 = CARTESIAN_POINT ( 'NONE',  ( 42.38452918213188525, 59.09948385550240602, -2.450534656007040013 ) ) ;
#12299 = DIRECTION ( 'NONE',  ( 1.000000000000000000, -0.000000000000000000, -0.000000000000000000 ) ) ;
#12300 = CARTESIAN_POINT ( 'NONE',  ( -12.99038105676659427, -12.50000000000003020, 9.000000000000000000 ) ) ;
#12301 = CARTESIAN_POINT ( 'NONE',  ( 43.18075615816989199, 51.19948385550240744, -4.924951120819313743 ) ) ;
#12302 = ORIENTED_EDGE ( 'NONE', *, *, #12273, .F. ) ;
#12303 = ORIENTED_EDGE ( 'NONE', *, *, #2899, .F. ) ;
#12304 = ORIENTED_EDGE ( 'NONE', *, *, #12089, .F. ) ;
#12305 = EDGE_LOOP ( 'NONE', ( #6691, #10248 ) ) ;
#12306 = CARTESIAN_POINT ( 'NONE',  ( -6.473970235329672780E-16, -4.862606272033106691, -3.745885042887442395 ) ) ;
#12307 = CARTESIAN_POINT ( 'NONE',  ( -2.354826896168714434, -6.962563485461402024, -1.000000000000000000 ) ) ;
#12308 = CARTESIAN_POINT ( 'NONE',  ( 0.000000000000000000, 0.000000000000000000, -5.000000000000000000 ) ) ;
#12309 = CARTESIAN_POINT ( 'NONE',  ( 13.67449106481161003, -13.83491329190030861, 0.000000000000000000 ) ) ;
#12310 = B_SPLINE_CURVE_WITH_KNOTS ( 'NONE', 3,
 ( #13534, #805, #4916, #9128 ),
 .UNSPECIFIED., .F., .F.,
 ( 4, 4 ),
 ( 0.000000000000000000, 0.002452478801916376308 ),
 .UNSPECIFIED. ) ;
#12311 = CARTESIAN_POINT ( 'NONE',  ( 53.54508667620428497, 62.29948385550241596, 4.840751629271157874 ) ) ;
#12312 = CARTESIAN_POINT ( 'NONE',  ( 45.86712807150329496, 51.70051614449766220, 5.649768623646139964 ) ) ;
#12313 = CARTESIAN_POINT ( 'NONE',  ( 57.60143344285435774, 61.10051614449766788, 2.493737253992045044 ) ) ;
#12314 = CARTESIAN_POINT ( 'NONE',  ( -4.000000000000000000, 1.677772373332757194, -3.535253723897187506 ) ) ;
#12315 = CARTESIAN_POINT ( 'NONE',  ( 58.41169779390614281, 53.00051614449765935, 0.02388180880515032231 ) ) ;
#12316 = PRODUCT_DEFINITION ( 'UNKNOWN', '', #4855, #968 ) ;
#12318 = ORIENTED_EDGE ( 'NONE', *, *, #13444, .T. ) ;
#12317 = ORIENTED_EDGE ( 'NONE', *, *, #2433, .T. ) ;
#12319 = LINE ( 'NONE', #487, #6633 ) ;
#12320 = ORIENTED_EDGE ( 'NONE', *, *, #6947, .F. ) ;
#12321 = ORIENTED_EDGE ( 'NONE', *, *, #4901, .F. ) ;
#12322 = DIRECTION ( 'NONE',  ( 0.000000000000000000, 0.000000000000000000, 1.000000000000000000 ) ) ;
#12323 = CARTESIAN_POINT ( 'NONE',  ( -2.688821387764050996E-14, -4.618802153517012954, -0.4999999999999995559 ) ) ;
#12324 = APPLICATION_PROTOCOL_DEFINITION ( 'draft international standard', 'automotive_design', 1998, #11835 ) ;
#12325 = CARTESIAN_POINT ( 'NONE',  ( 51.97223112728254790, 46.39948385550240317, 5.992620115222778487 ) ) ;
#12326 = AXIS2_PLACEMENT_3D ( 'NONE', #12023, #6770, #10973 ) ;
#12327 = CARTESIAN_POINT ( 'NONE',  ( 52.25172492374522903, 57.59948385550240602, -7.007379884777227730 ) ) ;
#12328 = VECTOR ( 'NONE', #1130, 999.9999999999998863 ) ;
#12329 = LINE ( 'NONE', #8266, #3582 ) ;
#12330 = CARTESIAN_POINT ( 'NONE',  ( 4.000000000000003553, 0.000000000000000000, 0.000000000000000000 ) ) ;
#12331 = CARTESIAN_POINT ( 'NONE',  ( 6.445379721942638973, 2.463581311471617852, 5.110653333236676588 ) ) ;
#12332 = CARTESIAN_POINT ( 'NONE',  ( 47.70284917648459100, 49.60051614449763946, 6.992620115222796251 ) ) ;
#12333 = CARTESIAN_POINT ( 'NONE',  ( 55.71335778527780747, 54.09948385550241312, 1.832500667257165983 ) ) ;
#12334 = CARTESIAN_POINT ( 'NONE',  ( 7.336184427528458230, 0.000000000000000000, 0.000000000000000000 ) ) ;
#12335 = EDGE_CURVE ( 'NONE', #6584, #5823, #8945, .T. ) ;
#12336 = ORIENTED_EDGE ( 'NONE', *, *, #5326, .T. ) ;
#12337 = CIRCLE ( 'NONE', #7047, 0.4999999999999978351 ) ;
#12338 = ORIENTED_EDGE ( 'NONE', *, *, #4754, .T. ) ;
#12339 = ORIENTED_EDGE ( 'NONE', *, *, #9443, .T. ) ;
#12340 = CARTESIAN_POINT ( 'NONE',  ( 4.165266963751721008, -2.049631966911996006, -3.550066703508900190 ) ) ;
#12341 = VECTOR ( 'NONE', #10951, 1000.000000000000000 ) ;
#12342 = CARTESIAN_POINT ( 'NONE',  ( 0.000000000000000000, 0.000000000000000000, -1.000000000000000000 ) ) ;
#12343 = DIRECTION ( 'NONE',  ( -1.000000000000000000, 0.000000000000000000, 0.000000000000000000 ) ) ;
#12344 =( NAMED_UNIT ( * ) SI_UNIT ( $, .STERADIAN. ) SOLID_ANGLE_UNIT ( ) );
#12345 = CARTESIAN_POINT ( 'NONE',  ( 42.63976443033212860, 46.99948385550240459, 0.02388180880522514787 ) ) ;
#12346 = PLANE ( 'NONE',  #5393 ) ;
#12347 = EDGE_CURVE ( 'NONE', #245, #919, #3099, .T. ) ;
#12348 = EDGE_CURVE ( 'NONE', #11555, #12722, #10915, .T. ) ;
#12349 = DIRECTION ( 'NONE',  ( 0.000000000000000000, 0.000000000000000000, -1.000000000000000000 ) ) ;
#12350 = CARTESIAN_POINT ( 'NONE',  ( 50.02271294988506156, 44.50051614449765935, -6.000000000000000888 ) ) ;
#12351 = EDGE_CURVE ( 'NONE', #13245, #2677, #4975, .T. ) ;
#12352 = CARTESIAN_POINT ( 'NONE',  ( 2.000000000000000000, -0.8865213383406694847, 1.535500000000001419 ) ) ;
#12353 = CARTESIAN_POINT ( 'NONE',  ( 56.65037692655918988, 55.89948385550240317, -2.184720259617163762 ) ) ;
#12354 = CARTESIAN_POINT ( 'NONE',  ( 45.90387839640214196, 52.69948385550240033, 5.676469297603166098 ) ) ;
#12355 = EDGE_CURVE ( 'NONE', #6754, #10018, #10288, .T. ) ;
#12356 = VERTEX_POINT ( 'NONE', #4980 ) ;
#12357 = CARTESIAN_POINT ( 'NONE',  ( 56.65037692655918988, 49.89948385550240317, -2.184720259617163762 ) ) ;
#12358 = ORIENTED_EDGE ( 'NONE', *, *, #426, .F. ) ;
#12359 = PRODUCT_DEFINITION_FORMATION_WITH_SPECIFIED_SOURCE ( 'ANY', '', #11401, .NOT_KNOWN. ) ;
#12360 = LINE ( 'NONE', #8222, #3283 ) ;
#12361 = ORIENTED_EDGE ( 'NONE', *, *, #12656, .T. ) ;
#12362 = CARTESIAN_POINT ( 'NONE',  ( -3.333333333333332149, -2.694301256218264218, -3.300726591567082036 ) ) ;
#12363 = FACE_OUTER_BOUND ( 'NONE', #10587, .T. ) ;
#12364 = FACE_OUTER_BOUND ( 'NONE', #8064, .T. ) ;
#12365 = CARTESIAN_POINT ( 'NONE',  ( 44.30067958973594955, 62.10051614449765367, -1.875703265242155693 ) ) ;
#12366 = CARTESIAN_POINT ( 'NONE',  ( 4.000000000001088907, 1.658577278524410170, -3.531553309554541720 ) ) ;
#12367 = CARTESIAN_POINT ( 'NONE',  ( 50.02271294988513972, 58.49948385550241170, 8.000000000000001776 ) ) ;
#12368 = ADVANCED_FACE ( 'NONE', ( #5321 ), #11800, .F. ) ;
#12369 = CARTESIAN_POINT ( 'NONE',  ( 47.70284917648453415, 63.39948385550240317, -6.992620115222774047 ) ) ;
#12370 = CARTESIAN_POINT ( 'NONE',  ( 2.000000000000000000, 0.8865213383406715941, 1.535499999999999199 ) ) ;
#12371 = CARTESIAN_POINT ( 'NONE',  ( 49.97728705011486738, 51.49948385550240459, -8.000000000000001776 ) ) ;
#12372 = EDGE_LOOP ( 'NONE', ( #2963, #13128, #8848, #9286 ) ) ;
#12373 = ORIENTED_EDGE ( 'NONE', *, *, #2561, .T. ) ;
#12374 = ORIENTED_EDGE ( 'NONE', *, *, #7184, .T. ) ;
#12375 = CARTESIAN_POINT ( 'NONE',  ( -9.999999999999996447, 25.00000000000001776, -15.00000000000000000 ) ) ;
#12376 = DIRECTION ( 'NONE',  ( 1.734723475976806848E-16, 1.000000000000000000, 0.000000000000000000 ) ) ;
#12377 = AXIS2_PLACEMENT_3D ( 'NONE', #3879, #6856, #6926 ) ;
#12378 = FACE_OUTER_BOUND ( 'NONE', #13325, .T. ) ;
#12379 = PLANE ( 'NONE',  #11273 ) ;
#12380 = FACE_OUTER_BOUND ( 'NONE', #11895, .T. ) ;
#12381 = CARTESIAN_POINT ( 'NONE',  ( 46.45491332379572924, 63.29948385550240175, -4.840751629271157874 ) ) ;
#12382 = CARTESIAN_POINT ( 'NONE',  ( 47.74827507625470702, 56.40051614449766504, -7.007379884777204637 ) ) ;
#12383 = CARTESIAN_POINT ( 'NONE',  ( 54.72065718078918906, 56.70051614449766930, -6.458785618021089192 ) ) ;
#12384 = EDGE_CURVE ( 'NONE', #2660, #2658, #1069, .T. ) ;
#12385 = ADVANCED_FACE ( 'NONE', ( #183 ), #11607, .F. ) ;
#12386 = DIRECTION ( 'NONE',  ( 0.000000000000000000, 0.000000000000000000, -1.000000000000000000 ) ) ;
#12387 = CARTESIAN_POINT ( 'NONE',  ( 54.68390685589039890, 49.30051614449766362, 6.485486291978072693 ) ) ;
#12389 = ORIENTED_EDGE ( 'NONE', *, *, #13529, .T. ) ;
#12388 = VERTEX_POINT ( 'NONE', #5586 ) ;
#12390 = VERTEX_POINT ( 'NONE', #3171 ) ;
#12391 = EDGE_LOOP ( 'NONE', ( #4204, #793 ) ) ;
#12392 = FACE_OUTER_BOUND ( 'NONE', #13260, .T. ) ;
#12393 = DIRECTION ( 'NONE',  ( 1.000000000000000000, 3.469446951953615668E-16, -0.000000000000000000 ) ) ;
#12394 = CARTESIAN_POINT ( 'NONE',  ( 2.385244779468109755E-15, -20.00000000000000000, -9.999999999999994671 ) ) ;
#12395 = AXIS2_PLACEMENT_3D ( 'NONE', #366, #1461, #6742 ) ;
#12396 = CARTESIAN_POINT ( 'NONE',  ( 54.09612160359786515, 63.69948385550240744, -5.676469297603166098 ) ) ;
#12397 = CARTESIAN_POINT ( 'NONE',  ( 45.86712807150323812, 59.29948385550240175, -5.649768623646098220 ) ) ;
#12398 = DIRECTION ( 'NONE',  ( -1.000000000000000000, 0.000000000000000000, 0.000000000000000000 ) ) ;
#12399 = DIRECTION ( 'NONE',  ( -0.000000000000000000, -0.000000000000000000, 1.000000000000000000 ) ) ;
#12400 = DIRECTION ( 'NONE',  ( 1.000000000000000000, 0.000000000000000000, 0.000000000000000000 ) ) ;
#12401 = CARTESIAN_POINT ( 'NONE',  ( 56.65037692655921120, 51.10051614449766078, 2.184720259617097593 ) ) ;
#12402 = CARTESIAN_POINT ( 'NONE',  ( 44.88205777487398507, 53.19948385550240744, -3.688883143319540814 ) ) ;
#12403 = DIRECTION ( 'NONE',  ( -0.9768494444668812671, -0.2139279384389642935, 0.000000000000000000 ) ) ;
#12404 = ORIENTED_EDGE ( 'NONE', *, *, #3924, .F. ) ;
#12405 = VECTOR ( 'NONE', #3945, 1000.000000000000000 ) ;
#12406 = CARTESIAN_POINT ( 'NONE',  ( 50.00000000000000000, 40.00000000000000000, 4.000000000000003553 ) ) ;
#12407 = EDGE_CURVE ( 'NONE', #7344, #1304, #1580, .T. ) ;
#12408 = VERTEX_POINT ( 'NONE', #1143 ) ;
#12409 = ORIENTED_EDGE ( 'NONE', *, *, #2327, .F. ) ;
#12410 = CARTESIAN_POINT ( 'NONE',  ( 4.175326769692856210, -2.060699556488920337, -3.569236330973475813 ) ) ;
#12411 = FACE_OUTER_BOUND ( 'NONE', #8877, .T. ) ;
#12412 = CARTESIAN_POINT ( 'NONE',  ( 6.507056315241516842, -5.826803161468474102, 0.09231912136634916333 ) ) ;
#12413 = CARTESIAN_POINT ( 'NONE',  ( 55.94051828345050836, 47.79948385550240886, -4.345558710429104465 ) ) ;
#12414 = CARTESIAN_POINT ( 'NONE',  ( 2.482347295856823136E-15, -20.00000000000000000, -8.999999999999996447 ) ) ;
#12415 = VECTOR ( 'NONE', #9863, 1000.000000000000000 ) ;
#12416 = LINE ( 'NONE', #5246, #6208 ) ;
#12417 = CARTESIAN_POINT ( 'NONE',  ( 49.97728705011488870, 63.49948385550241170, -6.000000000000000888 ) ) ;
#12418 = CARTESIAN_POINT ( 'NONE',  ( -2.134523027080836115E-16, -0.3420925509533478404, -3.499999999999999112 ) ) ;
#12419 = CARTESIAN_POINT ( 'NONE',  ( 56.65037692655918988, 57.89948385550240317, -2.184720259617163762 ) ) ;
#12420 = CARTESIAN_POINT ( 'NONE',  ( 43.33558569842703179, 51.09948385550240602, -2.141517661632099223 ) ) ;
#12421 = VECTOR ( 'NONE', #13200, 1000.000000000000000 ) ;
#12422 = ORIENTED_EDGE ( 'NONE', *, *, #6451, .F. ) ;
#12423 = CARTESIAN_POINT ( 'NONE',  ( 54.09612160359786515, 47.69948385550240744, -5.676469297603166098 ) ) ;
#12424 = ORIENTED_EDGE ( 'NONE', *, *, #9057, .F. ) ;
#12425 = DIRECTION ( 'NONE',  ( 0.000000000000000000, 0.000000000000000000, -1.000000000000000000 ) ) ;
#12426 = ORIENTED_EDGE ( 'NONE', *, *, #7880, .T. ) ;
#12427 = CARTESIAN_POINT ( 'NONE',  ( -9.999999999999998224, 15.00000000000001776, 15.00000000000000000 ) ) ;
#12428 = AXIS2_PLACEMENT_3D ( 'NONE', #7055, #11333, #735 ) ;
#12429 = CARTESIAN_POINT ( 'NONE',  ( -0.9999999999999976685, -20.00000000000000000, 8.999999999999998224 ) ) ;
#12430 = CARTESIAN_POINT ( 'NONE',  ( 20.00000000000000000, -20.00000000000000000, -20.00000000000000000 ) ) ;
#12431 = CARTESIAN_POINT ( 'NONE',  ( 44.88205777487401349, 63.80051614449766362, 3.688883143319584779 ) ) ;
#12432 = DIRECTION ( 'NONE',  ( 0.000000000000000000, -9.783878858594328898E-16, -1.000000000000000000 ) ) ;
#12433 = CARTESIAN_POINT ( 'NONE',  ( 52.62207051974839089, 60.39948385550241028, 7.992620115222770494 ) ) ;
#12434 = PLANE ( 'NONE',  #11989 ) ;
#12435 = CARTESIAN_POINT ( 'NONE',  ( 52.62207051974839089, 52.39948385550241028, 7.992620115222770494 ) ) ;
#12436 = ORIENTED_EDGE ( 'NONE', *, *, #1949, .F. ) ;
#12437 = ORIENTED_EDGE ( 'NONE', *, *, #11155, .T. ) ;
#12438 = ORIENTED_EDGE ( 'NONE', *, *, #1514, .F. ) ;
#12439 = CARTESIAN_POINT ( 'NONE',  ( -62.49999999999997158, 32.50000000000001421, 15.00000000000000000 ) ) ;
#12440 = ADVANCED_FACE ( 'NONE', ( #10759 ), #4529, .T. ) ;
#12441 = EDGE_CURVE ( 'NONE', #10124, #3640, #2397, .T. ) ;
#12442 = SURFACE_STYLE_FILL_AREA ( #8243 ) ;
#12443 = CARTESIAN_POINT ( 'NONE',  ( 3.958484000407829217, 2.327740518749080056, -2.968235154689852440 ) ) ;
#12444 = CARTESIAN_POINT ( 'NONE',  ( 2.899426713160750069, -23.82535289025860337, -9.999999999999994671 ) ) ;
#12445 = DIRECTION ( 'NONE',  ( 1.000000000000000000, 0.000000000000000000, 0.000000000000000000 ) ) ;
#12446 = CARTESIAN_POINT ( 'NONE',  ( 44.91013252490152752, 64.79948385550240175, 3.727524721679198461 ) ) ;
#12447 = EDGE_CURVE ( 'NONE', #9673, #11391, #10559, .T. ) ;
#12448 = CARTESIAN_POINT ( 'NONE',  ( 44.03140696652198471, 55.80051614449765651, 4.306917132069485454 ) ) ;
#12449 = AXIS2_PLACEMENT_3D ( 'NONE', #9845, #6675, #6870 ) ;
#12450 = CARTESIAN_POINT ( 'NONE',  ( 43.18075615816994173, 61.80051614449766362, 4.924951120819380357 ) ) ;
#12451 = CARTESIAN_POINT ( 'NONE',  ( -4.203934362469166963, -1.640673743454851286, -3.598432614606932756 ) ) ;
#12452 = CARTESIAN_POINT ( 'NONE',  ( 57.61547081786810764, 50.90051614449765793, -2.450534656007114176 ) ) ;
#12454 = ORIENTED_EDGE ( 'NONE', *, *, #12355, .F. ) ;
#12453 = ORIENTED_EDGE ( 'NONE', *, *, #6034, .T. ) ;
#12455 =( BOUNDED_SURFACE ( )  B_SPLINE_SURFACE ( 3, 2, ( 
 ( #11394, #5186, #10355 ),
 ( #866, #9399, #652 ),
 ( #7329, #12291, #13592 ),
 ( #1773, #11320, #5118 ),
 ( #9118, #13520, #4068 ),
 ( #10286, #4139, #8360 ) ),
 .UNSPECIFIED., .F., .F., .F. ) 
 B_SPLINE_SURFACE_WITH_KNOTS ( ( 4, 2, 4 ),
 ( 3, 3 ),
 ( 0.01651732063679904258, 0.01857756227444016389, 0.02063780391208128520 ),
 ( 0.000000000000000000, 1.000000000000000000 ),
 .UNSPECIFIED. ) 
 GEOMETRIC_REPRESENTATION_ITEM ( )  RATIONAL_B_SPLINE_SURFACE ( (
 ( 1.000000000000000000, 0.8047781231227483234, 1.000000000000000000),
 ( 1.000000000000000000, 0.8123782108664983070, 1.000000000000000000),
 ( 1.000000000000000000, 0.8190665102133478648, 1.000000000000000000),
 ( 1.000000000000000000, 0.8192358432844011329, 1.000000000000000000),
 ( 1.000000000000000000, 0.8126132624435309371, 1.000000000000000000),
 ( 1.000000000000000000, 0.8047712436238877443, 1.000000000000000000) ) ) 
 REPRESENTATION_ITEM ( '' )  SURFACE ( )  );
#12456 = ORIENTED_EDGE ( 'NONE', *, *, #5620, .F. ) ;
#12457 = UNCERTAINTY_MEASURE_WITH_UNIT (LENGTH_MEASURE( 1.000000000000000082E-05 ), #1588, 'distance_accuracy_value', 'NONE');
#12458 = ORIENTED_EDGE ( 'NONE', *, *, #1426, .T. ) ;
#12459 = VECTOR ( 'NONE', #298, 1000.000000000000000 ) ;
#12460 = CARTESIAN_POINT ( 'NONE',  ( 6.534838248920899595, 5.903531555104835071, 8.098083288904839678E-18 ) ) ;
#12461 = CARTESIAN_POINT ( 'NONE',  ( 0.01055556052338940676, 4.084588180558400339, -2.925285743277528105 ) ) ;
#12462 = CIRCLE ( 'NONE', #2078, 15.00000000000000000 ) ;
#12463 = DIRECTION ( 'NONE',  ( -1.000000000000000000, 0.000000000000000000, 0.000000000000000000 ) ) ;
#12464 = APPLICATION_PROTOCOL_DEFINITION ( 'draft international standard', 'automotive_design', 1998, #6389 ) ;
#12465 = CARTESIAN_POINT ( 'NONE',  ( 52.29715082351547295, 62.39948385550239607, 6.992620115222774047 ) ) ;
#12466 = CARTESIAN_POINT ( 'NONE',  ( 56.66441430157296821, 58.09948385550240602, 2.141517661632100111 ) ) ;
#12467 = CARTESIAN_POINT ( 'NONE',  ( 54.13287192849671214, 60.70051614449766220, -5.649768623646139964 ) ) ;
#12468 = CARTESIAN_POINT ( 'NONE',  ( -74.99999999999997158, 40.00000000000001421, -4.999999999999984013 ) ) ;
#12469 = VECTOR ( 'NONE', #2543, 1000.000000000000000 ) ;
#12470 = CARTESIAN_POINT ( 'NONE',  ( -62.49999999999997158, 45.00000000000001421, 15.00000000000000000 ) ) ;
#12471 = DIRECTION ( 'NONE',  ( 0.000000000000000000, 0.000000000000000000, -1.000000000000000000 ) ) ;
#12472 = EDGE_CURVE ( 'NONE', #6641, #5304, #328, .T. ) ;
#12473 = CARTESIAN_POINT ( 'NONE',  ( 47.70284917648459100, 51.60051614449765367, 6.992620115222796251 ) ) ;
#12474 = CARTESIAN_POINT ( 'NONE',  ( 44.28664221472220675, 51.09948385550240602, -1.832500667257165317 ) ) ;
#12475 = CARTESIAN_POINT ( 'NONE',  ( 1.267864665261691752E-11, -20.00000000000000000, 9.999999999999998224 ) ) ;
#12476 = VERTEX_POINT ( 'NONE', #12894 ) ;
#12477 = DIRECTION ( 'NONE',  ( 1.000000000000000000, 0.000000000000000000, -0.000000000000000000 ) ) ;
#12478 = ORIENTED_EDGE ( 'NONE', *, *, #7115, .T. ) ;
#12479 = VERTEX_POINT ( 'NONE', #9732 ) ;
#12480 = CARTESIAN_POINT ( 'NONE',  ( 3.333333333333332593, 2.694301256218250007, -3.300726591567078483 ) ) ;
#12481 = LINE ( 'NONE', #13367, #3212 ) ;
#12482 = EDGE_CURVE ( 'NONE', #9288, #7686, #2186, .T. ) ;
#12483 = EDGE_CURVE ( 'NONE', #9289, #1050, #5209, .T. ) ;
#12484 = CARTESIAN_POINT ( 'NONE',  ( 6.092449800118536096, -4.833012432206597708, -1.628976913806147397 ) ) ;
#12485 =( NAMED_UNIT ( * ) PLANE_ANGLE_UNIT ( ) SI_UNIT ( $, .RADIAN. ) );
#12486 = CARTESIAN_POINT ( 'NONE',  ( -3.455068668934486276, 2.624017327439035707, -3.316620875263955437 ) ) ;
#12487 = CARTESIAN_POINT ( 'NONE',  ( 51.97223112728254790, 64.39948385550239607, 5.992620115222778487 ) ) ;
#12488 = DIRECTION ( 'NONE',  ( -0.000000000000000000, -0.000000000000000000, 1.000000000000000000 ) ) ;
#12489 = CARTESIAN_POINT ( 'NONE',  ( 44.03140696652192787, 65.19948385550240744, -4.306917132069425058 ) ) ;
#12490 = CARTESIAN_POINT ( 'NONE',  ( 47.70284917648453415, 53.39948385550238186, -6.992620115222774047 ) ) ;
#12491 = EDGE_LOOP ( 'NONE', ( #2248, #11589, #10924, #5877 ) ) ;
#12492 = CARTESIAN_POINT ( 'NONE',  ( 45.86712807150323812, 53.29948385550240886, -5.649768623646098220 ) ) ;
#12493 = PRODUCT_DEFINITION ( 'UNKNOWN', '', #11252, #2926 ) ;
#12494 = ORIENTED_EDGE ( 'NONE', *, *, #12407, .T. ) ;
#12495 = DIRECTION ( 'NONE',  ( 1.000000000000000000, 0.000000000000000000, 0.000000000000000000 ) ) ;
#12496 = ORIENTED_EDGE ( 'NONE', *, *, #9897, .T. ) ;
#12497 = CARTESIAN_POINT ( 'NONE',  ( 4.165266963751721896, 2.049631966911991565, 3.550066703508901078 ) ) ;
#12498 = LINE ( 'NONE', #13453, #5630 ) ;
#12499 = CARTESIAN_POINT ( 'NONE',  ( 47.74827507625477807, 48.59948385550239891, 7.007379884777229506 ) ) ;
#12500 = CIRCLE ( 'NONE', #12711, 2.149999999999999023 ) ;
#12501 = CARTESIAN_POINT ( 'NONE',  ( 52.25172492374527877, 45.40051614449766504, 7.007379884777203749 ) ) ;
#12502 = CARTESIAN_POINT ( 'NONE',  ( 6.445127866599364097, -3.194847394660946360, 4.687657648742338701 ) ) ;
#12503 = CARTESIAN_POINT ( 'NONE',  ( 44.03140696652192787, 47.19948385550240744, -4.306917132069425058 ) ) ;
#12504 = CIRCLE ( 'NONE', #3247, 3.500000000000000000 ) ;
#12505 = DIRECTION ( 'NONE',  ( -1.000000000000000000, -0.000000000000000000, -0.000000000000000000 ) ) ;
#12506 = DIRECTION ( 'NONE',  ( 0.000000000000000000, 0.000000000000000000, -1.000000000000000000 ) ) ;
#12507 = CARTESIAN_POINT ( 'NONE',  ( 50.02271294988513972, 50.49948385550239749, 8.000000000000001776 ) ) ;
#12508 = B_SPLINE_CURVE_WITH_KNOTS ( 'NONE', 3,
 ( #9613, #9348, #12585, #4019, #10579, #2071, #3116, #1085 ),
 .UNSPECIFIED., .F., .F.,
 ( 4, 2, 2, 4 ),
 ( 1.228285202167177233E-19, 0.001493104274552340370, 0.002986208549104680306, 0.005972417098209360613 ),
 .UNSPECIFIED. ) ;
#12509 = ORIENTED_EDGE ( 'NONE', *, *, #6451, .T. ) ;
#12510 = ORIENTED_EDGE ( 'NONE', *, *, #13451, .T. ) ;
#12511 = VERTEX_POINT ( 'NONE', #3239 ) ;
#12512 = CARTESIAN_POINT ( 'NONE',  ( -74.99999999999998579, -2.602085213965210642E-14, 0.000000000000000000 ) ) ;
#12513 =( LENGTH_UNIT ( ) NAMED_UNIT ( * ) SI_UNIT ( .MILLI., .METRE. ) );
#12514 = FACE_OUTER_BOUND ( 'NONE', #1983, .T. ) ;
#12515 = CARTESIAN_POINT ( 'NONE',  ( 4.197393957002303999, 7.772902908466098641E-14, -3.503767560748929810 ) ) ;
#12516 = CARTESIAN_POINT ( 'NONE',  ( 30.00000000000000355, 0.000000000000000000, -10.00000000000000000 ) ) ;
#12517 = CARTESIAN_POINT ( 'NONE',  ( 55.71335778527780036, 50.90051614449765793, -1.832500667257213056 ) ) ;
#12518 = CARTESIAN_POINT ( 'NONE',  ( 52.29715082351539479, 58.60051614449766078, -6.992620115222796251 ) ) ;
#12519 = ADVANCED_FACE ( 'NONE', ( #4543 ), #10274, .T. ) ;
#12520 = CARTESIAN_POINT ( 'NONE',  ( 47.37792948025170858, 61.60051614449765367, 7.992620115222797139 ) ) ;
#12521 = CARTESIAN_POINT ( 'NONE',  ( -4.197477534772231955, 0.8522413273724368521, -3.505042416683225692 ) ) ;
#12522 = ADVANCED_FACE ( 'NONE', ( #10630 ), #2534, .T. ) ;
#12523 = EDGE_CURVE ( 'NONE', #7673, #9377, #8952, .T. ) ;
#12524 = CARTESIAN_POINT ( 'NONE',  ( 58.41169779390614281, 49.00051614449765935, 0.02388180880515032231 ) ) ;
#12525 = EDGE_CURVE ( 'NONE', #651, #13554, #11732, .T. ) ;
#12527 = ORIENTED_EDGE ( 'NONE', *, *, #10320, .F. ) ;
#12526 = EDGE_LOOP ( 'NONE', ( #3057, #8010, #5547, #595 ) ) ;
#12528 = ORIENTED_EDGE ( 'NONE', *, *, #6628, .T. ) ;
#12529 = ORIENTED_EDGE ( 'NONE', *, *, #7795, .T. ) ;
#12530 = CARTESIAN_POINT ( 'NONE',  ( 12.50000000000000000, 15.00000000000001776, 9.000000000000000000 ) ) ;
#12531 = EDGE_CURVE ( 'NONE', #2384, #439, #3704, .T. ) ;
#12532 = CARTESIAN_POINT ( 'NONE',  ( -4.999999999999998224, -20.00000000000000000, -9.999999999999994671 ) ) ;
#12533 = CARTESIAN_POINT ( 'NONE',  ( 0.000000000000000000, 4.330127018922190096, -2.500000000000006217 ) ) ;
#12534 = CARTESIAN_POINT ( 'NONE',  ( 49.99999999999997158, 65.00000000000002842, -7.000000000000000888 ) ) ;
#12535 = CARTESIAN_POINT ( 'NONE',  ( 43.33558569842703179, 61.09948385550240602, -2.141517661632099223 ) ) ;
#12536 = CARTESIAN_POINT ( 'NONE',  ( 62.50000000000000000, 20.00000000000001421, -9.999999999999998224 ) ) ;
#12537 = CARTESIAN_POINT ( 'NONE',  ( 47.74827507625469281, 62.40051614449766504, -7.007379884777203749 ) ) ;
#12538 = AXIS2_PLACEMENT_3D ( 'NONE', #10858, #13064, #4505 ) ;
#12539 = LINE ( 'NONE', #9568, #11748 ) ;
#12540 = DIRECTION ( 'NONE',  ( -0.000000000000000000, -0.000000000000000000, 1.000000000000000000 ) ) ;
#12541 = EDGE_CURVE ( 'NONE', #4606, #8295, #10490, .T. ) ;
#12542 =( BOUNDED_SURFACE ( )  B_SPLINE_SURFACE ( 3, 2, ( 
 ( #2466, #9933, #1554, #3651, #6703, #6973, #5804, #4692, #11176, #11943, #2673, #4824, #1418, #7936, #2533, #5665, #12218, #4552, #10000, #1696, #8972, #7873, #4760, #6765, #9039, #387, #12082, #4624, #1483, #2602, #3515, #6829, #13170, #3712, #12968, #6902, #10067, #1626, #13237, #8840, #3783, #8007, #2748, #327, #11035, #7739, #10968, #452, #4063, #10211, #4971, #3919, #9320, #5182, #3991, #8216, #12420, #8145, #12561, #2885, #9394, #7036, #646, #792, #4897, #8079, #7250, #10417, #2958, #11246, #9113, #9182, #12354, #6009, #13308, #3853, #10139, #719, #2817, #12490, #13442, #13376, #7107, #12285, #11316, #7183, #1981, #934, #13587, #1838, #6229, #3025, #6088, #4134, #11390, #3093, #10282, #7326, #1767, #5041, #9250, #11536, #1911, #6154, #8356, #2048, #10349, #861, #5111, #13513, #8289, #11456, #7517, #5384, #12628, #12885, #11724, #10624, #3432, #4201, #8621, #10754, #3163, #176, #46, #7389, #4464, #10488, #2244, #7654, #1206, #9591, #6491, #4271, #1261, #11602, #4333, #8425, #7454, #11792, #5453, #1132, #8690, #7585, #9653, #10692, #4394, #11658, #2178, #243, #9521, #113, #8489, #12818, #6426, #11859, #3361, #6296, #8554, #5512, #9452, #1001, #12750, #2315, #5251, #6553, #9723, #2113, #13652, #6361, #10553, #3294, #1064, #5316, #12692, #3232, #13022, #13155, #3565, #501, #7920, #9916, #8756, #4808, #307, #2446, #13219, #1539, #9788, #1398, #12132, #2656, #4535, #5716, #3766, #6685, #7721, #6880, #7788, #564, #8957 ),
 ( #9854, #5787, #11090, #437, #4670, #8894, #373, #9022, #8822, #1605, #12950, #6615, #6750, #10815, #3495, #3697, #5855, #13089, #11924, #1332, #5650, #4604, #10883, #5579, #12000, #2379, #2517, #10953, #4741, #3635, #1469, #7856, #12067, #2586, #6813, #10049, #7988, #11018, #9981, #8270, #838, #703, #4046, #9232, #5168, #3903, #916, #4883, #12268, #3836, #9372, #3970, #1749, #11439, #7236, #13360, #12474, #9093, #11229, #629, #8128, #13428, #11299, #13292, #13572, #8200, #2868, #4117, #10118, #5094, #3008, #8062, #6138, #5994, #2801, #10403, #2729, #12402, #11159, #10195, #4954, #7017, #6953, #1677, #12200, #9167, #12333, #9302, #1822, #7091, #6068, #5920, #10266, #2940, #1963, #6207, #775, #5026, #7164, #13496, #11374, #1893, #10332, #1246, #27, #10736, #983, #8406, #13634, #5496, #92, #11583, #7568, #3346, #9503, #8602, #5235, #7374, #10469, #4250, #9572, #7438, #9436, #9704, #4317, #12672, #230, #6280, #10676, #12803, #4183, #2228, #2097, #12611, #6537, #12545, #8537, #8341, #3277, #11643, #12735, #6343, #11776, #3144, #6409, #10538, #8469, #162, #7500, #3215, #3074, #9638, #11707, #6472, #1184, #2161, #10606, #2297, #1046, #1114, #5299, #5436, #5367, #7308, #4379, #11516, #2033, #11841, #2361, #6598, #4447, #1316, #5562, #10797, #9772, #12869, #8674, #3414, #7637, #11243, #12417, #858, #1692, #9110, #11387, #3849, #12282, #1764, #2955, #12487, #11313, #1835, #6084, #6006, #6227, #10208, #3022, #643, #8004, #8142, #12215 ),
 ( #12350, #2814, #2744, #10279, #716, #5108, #2882, #8285, #4967, #9316, #13305, #789, #3987, #10414, #3780, #1908, #7032, #13510, #5038, #6151, #3916, #6970, #13373, #9179, #13439, #7247, #9247, #10346, #8213, #4060, #11453, #7104, #4894, #8076, #7179, #11173, #1978, #930, #5179, #9389, #5934, #10136, #8353, #2108, #9648, #1256, #7513, #6486, #7449, #3090, #7323, #11596, #12745, #13647, #2311, #1128, #5380, #6550, #9586, #5509, #11654, #8617, #11533, #10750, #2174, #2241, #7581, #5449, #109, #6292, #10687, #172, #11720, #6422, #4328, #1202, #1060, #3159, #10549, #4389, #5312, #12814, #3357, #10620, #10483, #13584, #2045, #4197, #4131, #3290, #997, #12624, #11786, #12558, #5247, #3227, #9448, #8421, #7385, #6357, #9516, #42, #8550, #4267, #8484, #12687, #3427, #10879, #1393, #8751, #2442, #5711, #12880, #11085, #12127, #433, #10949, #13018, #13151, #8817, #4460, #9977, #7650, #5645, #7852, #9851, #8888, #11855, #12947, #5782, #496, #2375, #3559, #1601, #9784, #1327, #4736, #369, #7916, #11995, #8953, #3693, #2652, #6609, #4600, #7784, #3492, #6681, #9912, #10811, #9718, #6876, #4666, #1465, #2512, #240, #6746, #8686, #5575, #302, #13085, #12063, #3629, #4531, #7715, #2582, #11920, #6809, #11014, #1535, #5786, #2516, #9980, #7919, #2728, #3696, #8893, #9915, #3564, #13088, #11089, #5919, #4882, #3835, #436, #10117, #6952, #2585, #628, #1604, #7016, #500, #2800, #6749, #4669, #5715, #11228, #5854, #3634, #13291, #9092 ),
 ( #6812, #8061, #1748, #7987, #11158, #12131, #7787, #11999, #12066, #13218, #7855, #5993, #10048, #563, #372, #4807, #4603, #2655, #12267, #10952, #8821, #6879, #1676, #13021, #1468, #9021, #11017, #1538, #4740, #12199, #3765, #8956, #13154, #11373, #13427, #7163, #7307, #1892, #8340, #2032, #4045, #2867, #12610, #8127, #10265, #7373, #11438, #8199, #5234, #7090, #8269, #12332, #6137, #6279, #5167, #5093, #3143, #11515, #9371, #915, #10402, #10331, #837, #4182, #3969, #13495, #12401, #13571, #9301, #11582, #12544, #12473, #13359, #3007, #1962, #4116, #4953, #3073, #10468, #6206, #982, #11298, #9435, #13633, #8405, #2939, #2096, #10194, #1821, #6067, #702, #774, #5025, #7235, #9166, #3902, #9231, #4378, #161, #91, #8742, #12734, #5561, #3214, #10537, #8601, #3413, #6471, #9501, #1045, #7699, #1183, #5366, #5298, #12802, #3276, #7636, #6342, #10735, #6597, #11840, #11642, #3345, #6536, #12936, #26, #228, #9571, #2360, #7567, #4446, #10675, #4249, #2227, #4316, #2296, #9771, #11775, #12868, #1245, #8673, #1314, #8536, #7437, #2160, #7499, #8468, #11705, #10796, #6408, #5495, #292, #12671, #10605, #5435, #4518, #11907, #3480, #1113, #9703, #9637, #5631, #418, #1590, #2502, #4864, #3683, #7906, #9078, #12116, #8040, #9968, #11142, #9839, #2639, #1524, #8803, #13276, #6865, #6799, #3823, #359, #4794, #6934, #13003, #10035, #9901, #3547, #611, #6668, #11070, #2430, #5836, #5769, #549, #4655, #1660, #7773, #485, #4587, #3619 ),
 ( #7842, #5700, #13075, #13201, #12053, #9004, #7971, #4726, #11984, #10868, #6735, #10937, #1383, #3751, #1454, #8876, #12188, #2709, #2572, #8944, #11000, #13142, #5904, #10102, #13407, #10452, #819, #8321, #11495, #964, #5978, #3953, #8181, #11282, #5004, #8252, #1732, #13618, #5219, #2992, #13476, #1876, #2012, #11353, #7004, #12524, #10313, #9356, #12387, #10179, #11209, #4162, #7146, #1805, #684, #5073, #9216, #13551, #12252, #7216, #3053, #4100, #3885, #9285, #12452, #9421, #2784, #6187, #6050, #7285, #4028, #10382, #2921, #4936, #6118, #10243, #11419, #6262, #1940, #5148, #894, #9148, #13340, #756, #8112, #12315, #2849, #7073, #10586, #2274, #5, #143, #209, #11567, #6454, #6327, #9552, #4429, #3327, #3262, #10780, #9682, #7545, #12784, #8581, #76, #4297, #2343, #11628, #11688, #2143, #11757, #8520, #1299, #6521, #10655, #2079, #2208, #9619, #10719, #3122, #1231, #8652, #4362, #5478, #10518, #12849, #3395, #7617, #6388, #11822, #6581, #1031, #4229, #5543, #8450, #3194, #1096, #9754, #275, #1168, #5416, #8385, #5345, #12592, #12720, #7356, #5279, #9482, #12655, #7422, #7482, #3668, #4775, #6782, #5612, #3463, #3531, #6720, #342, #8725, #9882, #6653, #403, #12037, #6847, #7823, #12985, #4568, #7682, #7755, #1501, #10017, #8989, #7955, #8786, #534, #11052, #10920, #13186, #5750, #11122, #4638, #6917, #10849, #11962, #9823, #1643, #9949, #2484, #3727, #12168, #5682, #2691, #1367, #1433, #8857, #13054, #469, #3600, #2552 ),
 ( #5887, #10982, #12097, #4709, #8929, #10086, #12918, #13126, #4496, #7891, #2618, #1571, #5820, #11890, #2412, #2976, #2833, #6169, #11337, #7268, #6033, #3040, #6986, #663, #5960, #11478, #6105, #3869, #13536, #9339, #1786, #879, #11192, #13321, #2766, #10227, #1856, #13393, #1713, #2000, #10298, #4990, #6245, #12232, #7201, #5129, #10158, #8237, #8096, #4917, #12507, #4844, #806, #593, #9270, #3937, #5057, #12301, #4083, #9130, #12371, #7056, #737, #10369, #13461, #9200, #9058, #1925, #4010, #12435, #11406, #8166, #2904, #8306, #11267, #7128, #13254, #3802, #8023, #12839, #8569, #12707, #13605, #64, #11673, #9609, #5204, #130, #2262, #2196, #5402, #12576, #12771, #4352, #6439, #4216, #3314, #7535, #8371, #2066, #11743, #10504, #5266, #8437, #6508, #5468, #4284, #8507, #3250, #12644, #3381, #3178, #9671, #7340, #949, #10710, #1221, #10569, #196, #4418, #7470, #11552, #9407, #9466, #7408, #6313, #4147, #2131, #3111, #6374, #10643, #8637, #1154, #6418, #1017, #11616, #1078, #7602, #11810, #2331, #10439, #5333, #9537, #9743, #8974, #388, #8912, #519, #12083, #2535, #12906, #13110, #6831, #4693, #4625, #10969, #3652, #7740, #9806, #3516, #7875, #11946, #2604, #11037, #8842, #3448, #13171, #4484, #6638, #3713, #5734, #259, #5598, #1556, #5806, #8706, #9869, #7938, #10835, #11876, #10001, #2468, #4762, #13040, #12151, #6570, #10768, #7671, #6705, #10899, #329, #12970, #6767, #2398, #1284, #5530, #1485, #7808, #3584, #1354, #5667 ),
 ( #12019, #4554, #8773, #1420, #9934, #455, #6903, #8081, #4826, #12288, #10215, #5043, #6013, #11178, #12219, #5873, #1698, #13378, #8220, #7187, #6156, #2750, #12423, #9253, #4900, #2960, #3921, #9326, #2819, #5114, #9041, #6974, #8009, #13517, #8149, #5941, #1913, #11392, #3855, #10352, #13239, #10140, #3785, #7040, #12357, #1769, #647, #4065, #2888, #11249, #8291, #578, #13445, #863, #9115, #10284, #13309, #721, #2676, #11108, #7111, #1627, #11318, #4974, #9184, #10070, #1841, #6091, #794, #3994, #9396, #3027, #6231, #4136, #7253, #11459, #13590, #1984, #12492, #10423, #938, #5184, #531, #5541, #12983, #3529, #10847, #4565, #7820, #1297, #13184, #4773, #2550, #13052, #1431, #1569, #10917, #6579, #12094, #9879, #8925, #11959, #9752, #10778, #3724, #6717, #1365, #273, #401, #8784, #13124, #11819, #6779, #2616, #3666, #3461, #8855, #12035, #8987, #2341, #5748, #5610, #7889, #4636, #9947, #2482, #4494, #7753, #9820, #10980, #5818, #5679, #4707, #1498, #467, #6844, #339, #8720, #12915, #3597, #7680, #11050, #10014, #11888, #2410, #6651, #11119, #2689, #10156, #4200, #9520, #1853, #1000, #1784, #1641, #5884, #5957, #7126, #8021, #10552, #9198, #13391, #1063, #3935, #45, #6029, #3162, #10084, #5315, #10225, #10296, #2112, #13651, #8163, #591, #5250, #8424, #6103, #734, #12369, #9451, #9127, #11189, #4915, #12627, #13319, #7388, #11601, #4988, #4841, #7953, #9055, #6360, #2902, #13252, #12165, #6915, #3799, #11332, #12229, #2763 ) ),
 .UNSPECIFIED., .T., .F., .T. ) 
 B_SPLINE_SURFACE_WITH_KNOTS ( ( 4, 3, 4 ),
 ( 3, 2, 2, 2, 2, 2, 2, 2, 2, 2, 2, 2, 2, 2, 2, 2, 2, 2, 2, 2, 2, 2, 2, 2, 2, 2, 2, 2, 2, 2, 2, 2, 2, 2, 2, 2, 2, 2, 2, 2, 2, 2, 2, 2, 2, 2, 2, 2, 2, 2, 2, 2, 2, 2, 2, 2, 2, 2, 2, 2, 2, 2, 2, 2, 2, 2, 2, 2, 2, 2, 2, 2, 2, 2, 2, 2, 2, 2, 2, 2, 2, 2, 2, 2, 2, 2, 2, 2, 2, 2, 2, 2, 2, 2, 2, 2, 2, 2, 2, 2, 3 ),
 ( 0.000000000000000000, 0.5000000000000000000, 1.000000000000000000 ),
 ( 0.000000000000000000, 0.01000000000000000021, 0.02000000000000000042, 0.02999999999999999889, 0.04000000000000000083, 0.05000000000000000278, 0.05999999999999999778, 0.07000000000000000666, 0.08000000000000000167, 0.08999999999999999667, 0.1000000000000000056, 0.1100000000000000006, 0.1199999999999999956, 0.1300000000000000044, 0.1400000000000000133, 0.1499999999999999944, 0.1600000000000000033, 0.1700000000000000122, 0.1799999999999999933, 0.1900000000000000022, 0.2000000000000000111, 0.2099999999999999922, 0.2200000000000000011, 0.2300000000000000100, 0.2399999999999999911, 0.2500000000000000000, 0.2600000000000000089, 0.2700000000000000178, 0.2800000000000000266, 0.2899999999999999800, 0.2999999999999999889, 0.3099999999999999978, 0.3200000000000000067, 0.3300000000000000155, 0.3400000000000000244, 0.3499999999999999778, 0.3599999999999999867, 0.3699999999999999956, 0.3800000000000000044, 0.3900000000000000133, 0.4000000000000000222, 0.4099999999999999756, 0.4199999999999999845, 0.4299999999999999933, 0.4400000000000000022, 0.4500000000000000111, 0.4600000000000000200, 0.4699999999999999734, 0.4799999999999999822, 0.4899999999999999911, 0.5000000000000000000, 0.5100000000000000089, 0.5200000000000000178, 0.5300000000000000266, 0.5400000000000000355, 0.5500000000000000444, 0.5600000000000000533, 0.5699999999999999512, 0.5799999999999999600, 0.5899999999999999689, 0.5999999999999999778, 0.6099999999999999867, 0.6199999999999999956, 0.6300000000000000044, 0.6400000000000000133, 0.6500000000000000222, 0.6600000000000000311, 0.6700000000000000400, 0.6800000000000000488, 0.6899999999999999467, 0.6999999999999999556, 0.7099999999999999645, 0.7199999999999999734, 0.7299999999999999822, 0.7399999999999999911, 0.7500000000000000000, 0.7600000000000000089, 0.7700000000000000178, 0.7800000000000000266, 0.7900000000000000355, 0.8000000000000000444, 0.8100000000000000533, 0.8199999999999999512, 0.8299999999999999600, 0.8399999999999999689, 0.8499999999999999778, 0.8599999999999999867, 0.8699999999999999956, 0.8800000000000000044, 0.8900000000000000133, 0.9000000000000000222, 0.9100000000000000311, 0.9200000000000000400, 0.9300000000000000488, 0.9399999999999999467, 0.9499999999999999556, 0.9599999999999999645, 0.9699999999999999734, 0.9799999999999999822, 0.9899999999999999911, 1.000000000000000000 ),
 .UNSPECIFIED. ) 
 GEOMETRIC_REPRESENTATION_ITEM ( )  RATIONAL_B_SPLINE_SURFACE ( (
 ( 1.000000000000000000, 0.9510565162951535312, 1.000000000000000000, 0.9510565162951535312, 1.000000000000000000, 0.9510565162951535312, 1.000000000000000000, 0.9510565162951535312, 1.000000000000000000, 0.9510565162951535312, 1.000000000000000000, 0.9510565162951535312, 1.000000000000000000, 0.9510565162951535312, 1.000000000000000000, 0.9510565162951535312, 1.000000000000000000, 0.9510565162951535312, 1.000000000000000000, 0.9510565162951535312, 1.000000000000000000, 0.9510565162951535312, 1.000000000000000000, 0.9510565162951535312, 1.000000000000000000, 0.9510565162951535312, 1.000000000000000000, 0.9510565162951535312, 1.000000000000000000, 0.9510565162951535312, 1.000000000000000000, 0.9510565162951535312, 1.000000000000000000, 0.9510565162951535312, 1.000000000000000000, 0.9510565162951535312, 1.000000000000000000, 0.9510565162951535312, 1.000000000000000000, 0.9510565162951535312, 1.000000000000000000, 0.9510565162951535312, 1.000000000000000000, 0.9510565162951535312, 1.000000000000000000, 0.9510565162951535312, 1.000000000000000000, 0.9510565162951535312, 1.000000000000000000, 0.9510565162951535312, 1.000000000000000000, 0.9510565162951535312, 1.000000000000000000, 0.9510565162951535312, 1.000000000000000000, 0.9510565162951535312, 1.000000000000000000, 0.9510565162951535312, 1.000000000000000000, 0.9510565162951535312, 1.000000000000000000, 0.9510565162951535312, 1.000000000000000000, 0.9510565162951535312, 1.000000000000000000, 0.9510565162951535312, 1.000000000000000000, 0.9510565162951535312, 1.000000000000000000, 0.9510565162951535312, 1.000000000000000000, 0.9510565162951535312, 1.000000000000000000, 0.9510565162951535312, 1.000000000000000000, 0.9510565162951535312, 1.000000000000000000, 0.9510565162951535312, 1.000000000000000000, 0.9510565162951535312, 1.000000000000000000, 0.9510565162951535312, 1.000000000000000000, 0.9510565162951535312, 1.000000000000000000, 0.9510565162951535312, 1.000000000000000000, 0.9510565162951535312, 1.000000000000000000, 0.9510565162951535312, 1.000000000000000000, 0.9510565162951535312, 1.000000000000000000, 0.9510565162951535312, 1.000000000000000000, 0.9510565162951535312, 1.000000000000000000, 0.9510565162951535312, 1.000000000000000000, 0.9510565162951535312, 1.000000000000000000, 0.9510565162951535312, 1.000000000000000000, 0.9510565162951535312, 1.000000000000000000, 0.9510565162951535312, 1.000000000000000000, 0.9510565162951535312, 1.000000000000000000, 0.9510565162951535312, 1.000000000000000000, 0.9510565162951535312, 1.000000000000000000, 0.9510565162951535312, 1.000000000000000000, 0.9510565162951535312, 1.000000000000000000, 0.9510565162951535312, 1.000000000000000000, 0.9510565162951535312, 1.000000000000000000, 0.9510565162951535312, 1.000000000000000000, 0.9510565162951535312, 1.000000000000000000, 0.9510565162951535312, 1.000000000000000000, 0.9510565162951535312, 1.000000000000000000, 0.9510565162951535312, 1.000000000000000000, 0.9510565162951535312, 1.000000000000000000, 0.9510565162951535312, 1.000000000000000000, 0.9510565162951535312, 1.000000000000000000, 0.9510565162951535312, 1.000000000000000000, 0.9510565162951535312, 1.000000000000000000, 0.9510565162951535312, 1.000000000000000000, 0.9510565162951535312, 1.000000000000000000, 0.9510565162951535312, 1.000000000000000000, 0.9510565162951535312, 1.000000000000000000, 0.9510565162951535312, 1.000000000000000000, 0.9510565162951535312, 1.000000000000000000, 0.9510565162951535312, 1.000000000000000000, 0.9510565162951535312, 1.000000000000000000, 0.9510565162951535312, 1.000000000000000000, 0.9510565162951535312, 1.000000000000000000, 0.9510565162951535312, 1.000000000000000000, 0.9510565162951535312, 1.000000000000000000, 0.9510565162951535312, 1.000000000000000000, 0.9510565162951535312, 1.000000000000000000, 0.9510565162951535312, 1.000000000000000000, 0.9510565162951535312, 1.000000000000000000, 0.9510565162951535312, 1.000000000000000000, 0.9510565162951535312, 1.000000000000000000, 0.9510565162951535312, 1.000000000000000000, 0.9510565162951535312, 1.000000000000000000, 0.9510565162951535312, 1.000000000000000000, 0.9510565162951535312, 1.000000000000000000, 0.9510565162951535312, 1.000000000000000000, 0.9510565162951535312, 1.000000000000000000, 0.9510565162951535312, 1.000000000000000000, 0.9510565162951535312, 1.000000000000000000, 0.9510565162951535312, 1.000000000000000000, 0.9510565162951535312, 1.000000000000000000, 0.9510565162951535312, 1.000000000000000000, 0.9510565162951535312, 1.000000000000000000),
 ( 0.3333333333333333703, 0.3170188387650512141, 0.3333333333333333703, 0.3170188387650512141, 0.3333333333333333703, 0.3170188387650512141, 0.3333333333333333703, 0.3170188387650512141, 0.3333333333333333703, 0.3170188387650512141, 0.3333333333333333703, 0.3170188387650512141, 0.3333333333333333703, 0.3170188387650512141, 0.3333333333333333703, 0.3170188387650512141, 0.3333333333333333703, 0.3170188387650512141, 0.3333333333333333703, 0.3170188387650512141, 0.3333333333333333703, 0.3170188387650512141, 0.3333333333333333703, 0.3170188387650512141, 0.3333333333333333703, 0.3170188387650512141, 0.3333333333333333703, 0.3170188387650512141, 0.3333333333333333703, 0.3170188387650512141, 0.3333333333333333703, 0.3170188387650512141, 0.3333333333333333703, 0.3170188387650512141, 0.3333333333333333703, 0.3170188387650512141, 0.3333333333333333703, 0.3170188387650512141, 0.3333333333333333703, 0.3170188387650512141, 0.3333333333333333703, 0.3170188387650512141, 0.3333333333333333703, 0.3170188387650512141, 0.3333333333333333703, 0.3170188387650512141, 0.3333333333333333703, 0.3170188387650512141, 0.3333333333333333703, 0.3170188387650512141, 0.3333333333333333703, 0.3170188387650512141, 0.3333333333333333703, 0.3170188387650512141, 0.3333333333333333703, 0.3170188387650512141, 0.3333333333333333703, 0.3170188387650512141, 0.3333333333333333703, 0.3170188387650512141, 0.3333333333333333703, 0.3170188387650512141, 0.3333333333333333703, 0.3170188387650512141, 0.3333333333333333703, 0.3170188387650512141, 0.3333333333333333703, 0.3170188387650512141, 0.3333333333333333703, 0.3170188387650512141, 0.3333333333333333703, 0.3170188387650512141, 0.3333333333333333703, 0.3170188387650512141, 0.3333333333333333703, 0.3170188387650512141, 0.3333333333333333703, 0.3170188387650512141, 0.3333333333333333703, 0.3170188387650512141, 0.3333333333333333703, 0.3170188387650512141, 0.3333333333333333703, 0.3170188387650512141, 0.3333333333333333703, 0.3170188387650512141, 0.3333333333333333703, 0.3170188387650512141, 0.3333333333333333703, 0.3170188387650512141, 0.3333333333333333703, 0.3170188387650512141, 0.3333333333333333703, 0.3170188387650512141, 0.3333333333333333703, 0.3170188387650512141, 0.3333333333333333703, 0.3170188387650512141, 0.3333333333333333703, 0.3170188387650512141, 0.3333333333333333703, 0.3170188387650512141, 0.3333333333333333703, 0.3170188387650512141, 0.3333333333333333703, 0.3170188387650512141, 0.3333333333333333703, 0.3170188387650512141, 0.3333333333333333703, 0.3170188387650512141, 0.3333333333333333703, 0.3170188387650512141, 0.3333333333333333703, 0.3170188387650512141, 0.3333333333333333703, 0.3170188387650512141, 0.3333333333333333703, 0.3170188387650512141, 0.3333333333333333703, 0.3170188387650512141, 0.3333333333333333703, 0.3170188387650512141, 0.3333333333333333703, 0.3170188387650512141, 0.3333333333333333703, 0.3170188387650512141, 0.3333333333333333703, 0.3170188387650512141, 0.3333333333333333703, 0.3170188387650512141, 0.3333333333333333703, 0.3170188387650512141, 0.3333333333333333703, 0.3170188387650512141, 0.3333333333333333703, 0.3170188387650512141, 0.3333333333333333703, 0.3170188387650512141, 0.3333333333333333703, 0.3170188387650512141, 0.3333333333333333703, 0.3170188387650512141, 0.3333333333333333703, 0.3170188387650512141, 0.3333333333333333703, 0.3170188387650512141, 0.3333333333333333703, 0.3170188387650512141, 0.3333333333333333703, 0.3170188387650512141, 0.3333333333333333703, 0.3170188387650512141, 0.3333333333333333703, 0.3170188387650512141, 0.3333333333333333703, 0.3170188387650512141, 0.3333333333333333703, 0.3170188387650512141, 0.3333333333333333703, 0.3170188387650512141, 0.3333333333333333703, 0.3170188387650512141, 0.3333333333333333703, 0.3170188387650512141, 0.3333333333333333703, 0.3170188387650512141, 0.3333333333333333703, 0.3170188387650512141, 0.3333333333333333703, 0.3170188387650512141, 0.3333333333333333703, 0.3170188387650512141, 0.3333333333333333703, 0.3170188387650512141, 0.3333333333333333703, 0.3170188387650512141, 0.3333333333333333703, 0.3170188387650512141, 0.3333333333333333703, 0.3170188387650512141, 0.3333333333333333703, 0.3170188387650512141, 0.3333333333333333703, 0.3170188387650512141, 0.3333333333333333703, 0.3170188387650512141, 0.3333333333333333703, 0.3170188387650512141, 0.3333333333333333703, 0.3170188387650512141, 0.3333333333333333703, 0.3170188387650512141, 0.3333333333333333703, 0.3170188387650512141, 0.3333333333333333703, 0.3170188387650512141, 0.3333333333333333703, 0.3170188387650512141, 0.3333333333333333703, 0.3170188387650512141, 0.3333333333333333703),
 ( 0.3333333333333333703, 0.3170188387650512141, 0.3333333333333333703, 0.3170188387650512141, 0.3333333333333333703, 0.3170188387650512141, 0.3333333333333333703, 0.3170188387650512141, 0.3333333333333333703, 0.3170188387650512141, 0.3333333333333333703, 0.3170188387650512141, 0.3333333333333333703, 0.3170188387650512141, 0.3333333333333333703, 0.3170188387650512141, 0.3333333333333333703, 0.3170188387650512141, 0.3333333333333333703, 0.3170188387650512141, 0.3333333333333333703, 0.3170188387650512141, 0.3333333333333333703, 0.3170188387650512141, 0.3333333333333333703, 0.3170188387650512141, 0.3333333333333333703, 0.3170188387650512141, 0.3333333333333333703, 0.3170188387650512141, 0.3333333333333333703, 0.3170188387650512141, 0.3333333333333333703, 0.3170188387650512141, 0.3333333333333333703, 0.3170188387650512141, 0.3333333333333333703, 0.3170188387650512141, 0.3333333333333333703, 0.3170188387650512141, 0.3333333333333333703, 0.3170188387650512141, 0.3333333333333333703, 0.3170188387650512141, 0.3333333333333333703, 0.3170188387650512141, 0.3333333333333333703, 0.3170188387650512141, 0.3333333333333333703, 0.3170188387650512141, 0.3333333333333333703, 0.3170188387650512141, 0.3333333333333333703, 0.3170188387650512141, 0.3333333333333333703, 0.3170188387650512141, 0.3333333333333333703, 0.3170188387650512141, 0.3333333333333333703, 0.3170188387650512141, 0.3333333333333333703, 0.3170188387650512141, 0.3333333333333333703, 0.3170188387650512141, 0.3333333333333333703, 0.3170188387650512141, 0.3333333333333333703, 0.3170188387650512141, 0.3333333333333333703, 0.3170188387650512141, 0.3333333333333333703, 0.3170188387650512141, 0.3333333333333333703, 0.3170188387650512141, 0.3333333333333333703, 0.3170188387650512141, 0.3333333333333333703, 0.3170188387650512141, 0.3333333333333333703, 0.3170188387650512141, 0.3333333333333333703, 0.3170188387650512141, 0.3333333333333333703, 0.3170188387650512141, 0.3333333333333333703, 0.3170188387650512141, 0.3333333333333333703, 0.3170188387650512141, 0.3333333333333333703, 0.3170188387650512141, 0.3333333333333333703, 0.3170188387650512141, 0.3333333333333333703, 0.3170188387650512141, 0.3333333333333333703, 0.3170188387650512141, 0.3333333333333333703, 0.3170188387650512141, 0.3333333333333333703, 0.3170188387650512141, 0.3333333333333333703, 0.3170188387650512141, 0.3333333333333333703, 0.3170188387650512141, 0.3333333333333333703, 0.3170188387650512141, 0.3333333333333333703, 0.3170188387650512141, 0.3333333333333333703, 0.3170188387650512141, 0.3333333333333333703, 0.3170188387650512141, 0.3333333333333333703, 0.3170188387650512141, 0.3333333333333333703, 0.3170188387650512141, 0.3333333333333333703, 0.3170188387650512141, 0.3333333333333333703, 0.3170188387650512141, 0.3333333333333333703, 0.3170188387650512141, 0.3333333333333333703, 0.3170188387650512141, 0.3333333333333333703, 0.3170188387650512141, 0.3333333333333333703, 0.3170188387650512141, 0.3333333333333333703, 0.3170188387650512141, 0.3333333333333333703, 0.3170188387650512141, 0.3333333333333333703, 0.3170188387650512141, 0.3333333333333333703, 0.3170188387650512141, 0.3333333333333333703, 0.3170188387650512141, 0.3333333333333333703, 0.3170188387650512141, 0.3333333333333333703, 0.3170188387650512141, 0.3333333333333333703, 0.3170188387650512141, 0.3333333333333333703, 0.3170188387650512141, 0.3333333333333333703, 0.3170188387650512141, 0.3333333333333333703, 0.3170188387650512141, 0.3333333333333333703, 0.3170188387650512141, 0.3333333333333333703, 0.3170188387650512141, 0.3333333333333333703, 0.3170188387650512141, 0.3333333333333333703, 0.3170188387650512141, 0.3333333333333333703, 0.3170188387650512141, 0.3333333333333333703, 0.3170188387650512141, 0.3333333333333333703, 0.3170188387650512141, 0.3333333333333333703, 0.3170188387650512141, 0.3333333333333333703, 0.3170188387650512141, 0.3333333333333333703, 0.3170188387650512141, 0.3333333333333333703, 0.3170188387650512141, 0.3333333333333333703, 0.3170188387650512141, 0.3333333333333333703, 0.3170188387650512141, 0.3333333333333333703, 0.3170188387650512141, 0.3333333333333333703, 0.3170188387650512141, 0.3333333333333333703, 0.3170188387650512141, 0.3333333333333333703, 0.3170188387650512141, 0.3333333333333333703, 0.3170188387650512141, 0.3333333333333333703, 0.3170188387650512141, 0.3333333333333333703, 0.3170188387650512141, 0.3333333333333333703, 0.3170188387650512141, 0.3333333333333333703, 0.3170188387650512141, 0.3333333333333333703, 0.3170188387650512141, 0.3333333333333333703, 0.3170188387650512141, 0.3333333333333333703, 0.3170188387650512141, 0.3333333333333333703),
 ( 1.000000000000000000, 0.9510565162951535312, 1.000000000000000000, 0.9510565162951535312, 1.000000000000000000, 0.9510565162951535312, 1.000000000000000000, 0.9510565162951535312, 1.000000000000000000, 0.9510565162951535312, 1.000000000000000000, 0.9510565162951535312, 1.000000000000000000, 0.9510565162951535312, 1.000000000000000000, 0.9510565162951535312, 1.000000000000000000, 0.9510565162951535312, 1.000000000000000000, 0.9510565162951535312, 1.000000000000000000, 0.9510565162951535312, 1.000000000000000000, 0.9510565162951535312, 1.000000000000000000, 0.9510565162951535312, 1.000000000000000000, 0.9510565162951535312, 1.000000000000000000, 0.9510565162951535312, 1.000000000000000000, 0.9510565162951535312, 1.000000000000000000, 0.9510565162951535312, 1.000000000000000000, 0.9510565162951535312, 1.000000000000000000, 0.9510565162951535312, 1.000000000000000000, 0.9510565162951535312, 1.000000000000000000, 0.9510565162951535312, 1.000000000000000000, 0.9510565162951535312, 1.000000000000000000, 0.9510565162951535312, 1.000000000000000000, 0.9510565162951535312, 1.000000000000000000, 0.9510565162951535312, 1.000000000000000000, 0.9510565162951535312, 1.000000000000000000, 0.9510565162951535312, 1.000000000000000000, 0.9510565162951535312, 1.000000000000000000, 0.9510565162951535312, 1.000000000000000000, 0.9510565162951535312, 1.000000000000000000, 0.9510565162951535312, 1.000000000000000000, 0.9510565162951535312, 1.000000000000000000, 0.9510565162951535312, 1.000000000000000000, 0.9510565162951535312, 1.000000000000000000, 0.9510565162951535312, 1.000000000000000000, 0.9510565162951535312, 1.000000000000000000, 0.9510565162951535312, 1.000000000000000000, 0.9510565162951535312, 1.000000000000000000, 0.9510565162951535312, 1.000000000000000000, 0.9510565162951535312, 1.000000000000000000, 0.9510565162951535312, 1.000000000000000000, 0.9510565162951535312, 1.000000000000000000, 0.9510565162951535312, 1.000000000000000000, 0.9510565162951535312, 1.000000000000000000, 0.9510565162951535312, 1.000000000000000000, 0.9510565162951535312, 1.000000000000000000, 0.9510565162951535312, 1.000000000000000000, 0.9510565162951535312, 1.000000000000000000, 0.9510565162951535312, 1.000000000000000000, 0.9510565162951535312, 1.000000000000000000, 0.9510565162951535312, 1.000000000000000000, 0.9510565162951535312, 1.000000000000000000, 0.9510565162951535312, 1.000000000000000000, 0.9510565162951535312, 1.000000000000000000, 0.9510565162951535312, 1.000000000000000000, 0.9510565162951535312, 1.000000000000000000, 0.9510565162951535312, 1.000000000000000000, 0.9510565162951535312, 1.000000000000000000, 0.9510565162951535312, 1.000000000000000000, 0.9510565162951535312, 1.000000000000000000, 0.9510565162951535312, 1.000000000000000000, 0.9510565162951535312, 1.000000000000000000, 0.9510565162951535312, 1.000000000000000000, 0.9510565162951535312, 1.000000000000000000, 0.9510565162951535312, 1.000000000000000000, 0.9510565162951535312, 1.000000000000000000, 0.9510565162951535312, 1.000000000000000000, 0.9510565162951535312, 1.000000000000000000, 0.9510565162951535312, 1.000000000000000000, 0.9510565162951535312, 1.000000000000000000, 0.9510565162951535312, 1.000000000000000000, 0.9510565162951535312, 1.000000000000000000, 0.9510565162951535312, 1.000000000000000000, 0.9510565162951535312, 1.000000000000000000, 0.9510565162951535312, 1.000000000000000000, 0.9510565162951535312, 1.000000000000000000, 0.9510565162951535312, 1.000000000000000000, 0.9510565162951535312, 1.000000000000000000, 0.9510565162951535312, 1.000000000000000000, 0.9510565162951535312, 1.000000000000000000, 0.9510565162951535312, 1.000000000000000000, 0.9510565162951535312, 1.000000000000000000, 0.9510565162951535312, 1.000000000000000000, 0.9510565162951535312, 1.000000000000000000, 0.9510565162951535312, 1.000000000000000000, 0.9510565162951535312, 1.000000000000000000, 0.9510565162951535312, 1.000000000000000000, 0.9510565162951535312, 1.000000000000000000, 0.9510565162951535312, 1.000000000000000000, 0.9510565162951535312, 1.000000000000000000, 0.9510565162951535312, 1.000000000000000000, 0.9510565162951535312, 1.000000000000000000, 0.9510565162951535312, 1.000000000000000000, 0.9510565162951535312, 1.000000000000000000, 0.9510565162951535312, 1.000000000000000000, 0.9510565162951535312, 1.000000000000000000, 0.9510565162951535312, 1.000000000000000000, 0.9510565162951535312, 1.000000000000000000, 0.9510565162951535312, 1.000000000000000000, 0.9510565162951535312, 1.000000000000000000),
 ( 0.3333333333333333703, 0.3170188387650512141, 0.3333333333333333703, 0.3170188387650512141, 0.3333333333333333703, 0.3170188387650512141, 0.3333333333333333703, 0.3170188387650512141, 0.3333333333333333703, 0.3170188387650512141, 0.3333333333333333703, 0.3170188387650512141, 0.3333333333333333703, 0.3170188387650512141, 0.3333333333333333703, 0.3170188387650512141, 0.3333333333333333703, 0.3170188387650512141, 0.3333333333333333703, 0.3170188387650512141, 0.3333333333333333703, 0.3170188387650512141, 0.3333333333333333703, 0.3170188387650512141, 0.3333333333333333703, 0.3170188387650512141, 0.3333333333333333703, 0.3170188387650512141, 0.3333333333333333703, 0.3170188387650512141, 0.3333333333333333703, 0.3170188387650512141, 0.3333333333333333703, 0.3170188387650512141, 0.3333333333333333703, 0.3170188387650512141, 0.3333333333333333703, 0.3170188387650512141, 0.3333333333333333703, 0.3170188387650512141, 0.3333333333333333703, 0.3170188387650512141, 0.3333333333333333703, 0.3170188387650512141, 0.3333333333333333703, 0.3170188387650512141, 0.3333333333333333703, 0.3170188387650512141, 0.3333333333333333703, 0.3170188387650512141, 0.3333333333333333703, 0.3170188387650512141, 0.3333333333333333703, 0.3170188387650512141, 0.3333333333333333703, 0.3170188387650512141, 0.3333333333333333703, 0.3170188387650512141, 0.3333333333333333703, 0.3170188387650512141, 0.3333333333333333703, 0.3170188387650512141, 0.3333333333333333703, 0.3170188387650512141, 0.3333333333333333703, 0.3170188387650512141, 0.3333333333333333703, 0.3170188387650512141, 0.3333333333333333703, 0.3170188387650512141, 0.3333333333333333703, 0.3170188387650512141, 0.3333333333333333703, 0.3170188387650512141, 0.3333333333333333703, 0.3170188387650512141, 0.3333333333333333703, 0.3170188387650512141, 0.3333333333333333703, 0.3170188387650512141, 0.3333333333333333703, 0.3170188387650512141, 0.3333333333333333703, 0.3170188387650512141, 0.3333333333333333703, 0.3170188387650512141, 0.3333333333333333703, 0.3170188387650512141, 0.3333333333333333703, 0.3170188387650512141, 0.3333333333333333703, 0.3170188387650512141, 0.3333333333333333703, 0.3170188387650512141, 0.3333333333333333703, 0.3170188387650512141, 0.3333333333333333703, 0.3170188387650512141, 0.3333333333333333703, 0.3170188387650512141, 0.3333333333333333703, 0.3170188387650512141, 0.3333333333333333703, 0.3170188387650512141, 0.3333333333333333703, 0.3170188387650512141, 0.3333333333333333703, 0.3170188387650512141, 0.3333333333333333703, 0.3170188387650512141, 0.3333333333333333703, 0.3170188387650512141, 0.3333333333333333703, 0.3170188387650512141, 0.3333333333333333703, 0.3170188387650512141, 0.3333333333333333703, 0.3170188387650512141, 0.3333333333333333703, 0.3170188387650512141, 0.3333333333333333703, 0.3170188387650512141, 0.3333333333333333703, 0.3170188387650512141, 0.3333333333333333703, 0.3170188387650512141, 0.3333333333333333703, 0.3170188387650512141, 0.3333333333333333703, 0.3170188387650512141, 0.3333333333333333703, 0.3170188387650512141, 0.3333333333333333703, 0.3170188387650512141, 0.3333333333333333703, 0.3170188387650512141, 0.3333333333333333703, 0.3170188387650512141, 0.3333333333333333703, 0.3170188387650512141, 0.3333333333333333703, 0.3170188387650512141, 0.3333333333333333703, 0.3170188387650512141, 0.3333333333333333703, 0.3170188387650512141, 0.3333333333333333703, 0.3170188387650512141, 0.3333333333333333703, 0.3170188387650512141, 0.3333333333333333703, 0.3170188387650512141, 0.3333333333333333703, 0.3170188387650512141, 0.3333333333333333703, 0.3170188387650512141, 0.3333333333333333703, 0.3170188387650512141, 0.3333333333333333703, 0.3170188387650512141, 0.3333333333333333703, 0.3170188387650512141, 0.3333333333333333703, 0.3170188387650512141, 0.3333333333333333703, 0.3170188387650512141, 0.3333333333333333703, 0.3170188387650512141, 0.3333333333333333703, 0.3170188387650512141, 0.3333333333333333703, 0.3170188387650512141, 0.3333333333333333703, 0.3170188387650512141, 0.3333333333333333703, 0.3170188387650512141, 0.3333333333333333703, 0.3170188387650512141, 0.3333333333333333703, 0.3170188387650512141, 0.3333333333333333703, 0.3170188387650512141, 0.3333333333333333703, 0.3170188387650512141, 0.3333333333333333703, 0.3170188387650512141, 0.3333333333333333703, 0.3170188387650512141, 0.3333333333333333703, 0.3170188387650512141, 0.3333333333333333703, 0.3170188387650512141, 0.3333333333333333703, 0.3170188387650512141, 0.3333333333333333703, 0.3170188387650512141, 0.3333333333333333703, 0.3170188387650512141, 0.3333333333333333703, 0.3170188387650512141, 0.3333333333333333703),
 ( 0.3333333333333333703, 0.3170188387650512141, 0.3333333333333333703, 0.3170188387650512141, 0.3333333333333333703, 0.3170188387650512141, 0.3333333333333333703, 0.3170188387650512141, 0.3333333333333333703, 0.3170188387650512141, 0.3333333333333333703, 0.3170188387650512141, 0.3333333333333333703, 0.3170188387650512141, 0.3333333333333333703, 0.3170188387650512141, 0.3333333333333333703, 0.3170188387650512141, 0.3333333333333333703, 0.3170188387650512141, 0.3333333333333333703, 0.3170188387650512141, 0.3333333333333333703, 0.3170188387650512141, 0.3333333333333333703, 0.3170188387650512141, 0.3333333333333333703, 0.3170188387650512141, 0.3333333333333333703, 0.3170188387650512141, 0.3333333333333333703, 0.3170188387650512141, 0.3333333333333333703, 0.3170188387650512141, 0.3333333333333333703, 0.3170188387650512141, 0.3333333333333333703, 0.3170188387650512141, 0.3333333333333333703, 0.3170188387650512141, 0.3333333333333333703, 0.3170188387650512141, 0.3333333333333333703, 0.3170188387650512141, 0.3333333333333333703, 0.3170188387650512141, 0.3333333333333333703, 0.3170188387650512141, 0.3333333333333333703, 0.3170188387650512141, 0.3333333333333333703, 0.3170188387650512141, 0.3333333333333333703, 0.3170188387650512141, 0.3333333333333333703, 0.3170188387650512141, 0.3333333333333333703, 0.3170188387650512141, 0.3333333333333333703, 0.3170188387650512141, 0.3333333333333333703, 0.3170188387650512141, 0.3333333333333333703, 0.3170188387650512141, 0.3333333333333333703, 0.3170188387650512141, 0.3333333333333333703, 0.3170188387650512141, 0.3333333333333333703, 0.3170188387650512141, 0.3333333333333333703, 0.3170188387650512141, 0.3333333333333333703, 0.3170188387650512141, 0.3333333333333333703, 0.3170188387650512141, 0.3333333333333333703, 0.3170188387650512141, 0.3333333333333333703, 0.3170188387650512141, 0.3333333333333333703, 0.3170188387650512141, 0.3333333333333333703, 0.3170188387650512141, 0.3333333333333333703, 0.3170188387650512141, 0.3333333333333333703, 0.3170188387650512141, 0.3333333333333333703, 0.3170188387650512141, 0.3333333333333333703, 0.3170188387650512141, 0.3333333333333333703, 0.3170188387650512141, 0.3333333333333333703, 0.3170188387650512141, 0.3333333333333333703, 0.3170188387650512141, 0.3333333333333333703, 0.3170188387650512141, 0.3333333333333333703, 0.3170188387650512141, 0.3333333333333333703, 0.3170188387650512141, 0.3333333333333333703, 0.3170188387650512141, 0.3333333333333333703, 0.3170188387650512141, 0.3333333333333333703, 0.3170188387650512141, 0.3333333333333333703, 0.3170188387650512141, 0.3333333333333333703, 0.3170188387650512141, 0.3333333333333333703, 0.3170188387650512141, 0.3333333333333333703, 0.3170188387650512141, 0.3333333333333333703, 0.3170188387650512141, 0.3333333333333333703, 0.3170188387650512141, 0.3333333333333333703, 0.3170188387650512141, 0.3333333333333333703, 0.3170188387650512141, 0.3333333333333333703, 0.3170188387650512141, 0.3333333333333333703, 0.3170188387650512141, 0.3333333333333333703, 0.3170188387650512141, 0.3333333333333333703, 0.3170188387650512141, 0.3333333333333333703, 0.3170188387650512141, 0.3333333333333333703, 0.3170188387650512141, 0.3333333333333333703, 0.3170188387650512141, 0.3333333333333333703, 0.3170188387650512141, 0.3333333333333333703, 0.3170188387650512141, 0.3333333333333333703, 0.3170188387650512141, 0.3333333333333333703, 0.3170188387650512141, 0.3333333333333333703, 0.3170188387650512141, 0.3333333333333333703, 0.3170188387650512141, 0.3333333333333333703, 0.3170188387650512141, 0.3333333333333333703, 0.3170188387650512141, 0.3333333333333333703, 0.3170188387650512141, 0.3333333333333333703, 0.3170188387650512141, 0.3333333333333333703, 0.3170188387650512141, 0.3333333333333333703, 0.3170188387650512141, 0.3333333333333333703, 0.3170188387650512141, 0.3333333333333333703, 0.3170188387650512141, 0.3333333333333333703, 0.3170188387650512141, 0.3333333333333333703, 0.3170188387650512141, 0.3333333333333333703, 0.3170188387650512141, 0.3333333333333333703, 0.3170188387650512141, 0.3333333333333333703, 0.3170188387650512141, 0.3333333333333333703, 0.3170188387650512141, 0.3333333333333333703, 0.3170188387650512141, 0.3333333333333333703, 0.3170188387650512141, 0.3333333333333333703, 0.3170188387650512141, 0.3333333333333333703, 0.3170188387650512141, 0.3333333333333333703, 0.3170188387650512141, 0.3333333333333333703, 0.3170188387650512141, 0.3333333333333333703, 0.3170188387650512141, 0.3333333333333333703, 0.3170188387650512141, 0.3333333333333333703, 0.3170188387650512141, 0.3333333333333333703, 0.3170188387650512141, 0.3333333333333333703),
 ( 1.000000000000000000, 0.9510565162951535312, 1.000000000000000000, 0.9510565162951535312, 1.000000000000000000, 0.9510565162951535312, 1.000000000000000000, 0.9510565162951535312, 1.000000000000000000, 0.9510565162951535312, 1.000000000000000000, 0.9510565162951535312, 1.000000000000000000, 0.9510565162951535312, 1.000000000000000000, 0.9510565162951535312, 1.000000000000000000, 0.9510565162951535312, 1.000000000000000000, 0.9510565162951535312, 1.000000000000000000, 0.9510565162951535312, 1.000000000000000000, 0.9510565162951535312, 1.000000000000000000, 0.9510565162951535312, 1.000000000000000000, 0.9510565162951535312, 1.000000000000000000, 0.9510565162951535312, 1.000000000000000000, 0.9510565162951535312, 1.000000000000000000, 0.9510565162951535312, 1.000000000000000000, 0.9510565162951535312, 1.000000000000000000, 0.9510565162951535312, 1.000000000000000000, 0.9510565162951535312, 1.000000000000000000, 0.9510565162951535312, 1.000000000000000000, 0.9510565162951535312, 1.000000000000000000, 0.9510565162951535312, 1.000000000000000000, 0.9510565162951535312, 1.000000000000000000, 0.9510565162951535312, 1.000000000000000000, 0.9510565162951535312, 1.000000000000000000, 0.9510565162951535312, 1.000000000000000000, 0.9510565162951535312, 1.000000000000000000, 0.9510565162951535312, 1.000000000000000000, 0.9510565162951535312, 1.000000000000000000, 0.9510565162951535312, 1.000000000000000000, 0.9510565162951535312, 1.000000000000000000, 0.9510565162951535312, 1.000000000000000000, 0.9510565162951535312, 1.000000000000000000, 0.9510565162951535312, 1.000000000000000000, 0.9510565162951535312, 1.000000000000000000, 0.9510565162951535312, 1.000000000000000000, 0.9510565162951535312, 1.000000000000000000, 0.9510565162951535312, 1.000000000000000000, 0.9510565162951535312, 1.000000000000000000, 0.9510565162951535312, 1.000000000000000000, 0.9510565162951535312, 1.000000000000000000, 0.9510565162951535312, 1.000000000000000000, 0.9510565162951535312, 1.000000000000000000, 0.9510565162951535312, 1.000000000000000000, 0.9510565162951535312, 1.000000000000000000, 0.9510565162951535312, 1.000000000000000000, 0.9510565162951535312, 1.000000000000000000, 0.9510565162951535312, 1.000000000000000000, 0.9510565162951535312, 1.000000000000000000, 0.9510565162951535312, 1.000000000000000000, 0.9510565162951535312, 1.000000000000000000, 0.9510565162951535312, 1.000000000000000000, 0.9510565162951535312, 1.000000000000000000, 0.9510565162951535312, 1.000000000000000000, 0.9510565162951535312, 1.000000000000000000, 0.9510565162951535312, 1.000000000000000000, 0.9510565162951535312, 1.000000000000000000, 0.9510565162951535312, 1.000000000000000000, 0.9510565162951535312, 1.000000000000000000, 0.9510565162951535312, 1.000000000000000000, 0.9510565162951535312, 1.000000000000000000, 0.9510565162951535312, 1.000000000000000000, 0.9510565162951535312, 1.000000000000000000, 0.9510565162951535312, 1.000000000000000000, 0.9510565162951535312, 1.000000000000000000, 0.9510565162951535312, 1.000000000000000000, 0.9510565162951535312, 1.000000000000000000, 0.9510565162951535312, 1.000000000000000000, 0.9510565162951535312, 1.000000000000000000, 0.9510565162951535312, 1.000000000000000000, 0.9510565162951535312, 1.000000000000000000, 0.9510565162951535312, 1.000000000000000000, 0.9510565162951535312, 1.000000000000000000, 0.9510565162951535312, 1.000000000000000000, 0.9510565162951535312, 1.000000000000000000, 0.9510565162951535312, 1.000000000000000000, 0.9510565162951535312, 1.000000000000000000, 0.9510565162951535312, 1.000000000000000000, 0.9510565162951535312, 1.000000000000000000, 0.9510565162951535312, 1.000000000000000000, 0.9510565162951535312, 1.000000000000000000, 0.9510565162951535312, 1.000000000000000000, 0.9510565162951535312, 1.000000000000000000, 0.9510565162951535312, 1.000000000000000000, 0.9510565162951535312, 1.000000000000000000, 0.9510565162951535312, 1.000000000000000000, 0.9510565162951535312, 1.000000000000000000, 0.9510565162951535312, 1.000000000000000000, 0.9510565162951535312, 1.000000000000000000, 0.9510565162951535312, 1.000000000000000000, 0.9510565162951535312, 1.000000000000000000, 0.9510565162951535312, 1.000000000000000000, 0.9510565162951535312, 1.000000000000000000, 0.9510565162951535312, 1.000000000000000000, 0.9510565162951535312, 1.000000000000000000, 0.9510565162951535312, 1.000000000000000000, 0.9510565162951535312, 1.000000000000000000, 0.9510565162951535312, 1.000000000000000000, 0.9510565162951535312, 1.000000000000000000) ) ) 
 REPRESENTATION_ITEM ( '' )  SURFACE ( )  );
#12543 = CARTESIAN_POINT ( 'NONE',  ( 2.000000000000000000, 0.000000000000000000, 0.000000000000000000 ) ) ;
#12544 = CARTESIAN_POINT ( 'NONE',  ( 49.97728705011495265, 51.50051614449765935, 7.000000000000000888 ) ) ;
#12545 = CARTESIAN_POINT ( 'NONE',  ( 43.69122665457040000, 58.99948385550239749, 0.02388180880521036456 ) ) ;
#12546 = DIRECTION ( 'NONE',  ( 1.000000000000000000, 0.000000000000000000, -0.000000000000000000 ) ) ;
#12547 = ORIENTED_EDGE ( 'NONE', *, *, #8645, .T. ) ;
#12548 = CARTESIAN_POINT ( 'NONE',  ( -62.49999999999997158, 45.00000000000001421, 9.999999999999998224 ) ) ;
#12549 = ORIENTED_EDGE ( 'NONE', *, *, #341, .T. ) ;
#12550 = VERTEX_POINT ( 'NONE', #8830 ) ;
#12551 = CARTESIAN_POINT ( 'NONE',  ( 6.534224484704324709, 2.950930484791589148, 5.111161529262913561 ) ) ;
#12552 = AXIS2_PLACEMENT_3D ( 'NONE', #12956, #9987, #3641 ) ;
#12553 = CARTESIAN_POINT ( 'NONE',  ( 6.327632967270859332, 5.346704644972003706, -0.7392359018481428068 ) ) ;
#12554 = CYLINDRICAL_SURFACE ( 'NONE', #2224, 4.799999999999999822 ) ;
#12555 = FILL_AREA_STYLE ('',( #6079 ) ) ;
#12556 = LINE ( 'NONE', #7175, #6176 ) ;
#12557 = LINE ( 'NONE', #10413, #2420 ) ;
#12558 = CARTESIAN_POINT ( 'NONE',  ( 44.88205777487401349, 53.80051614449766362, 3.688883143319584779 ) ) ;
#12559 = DIRECTION ( 'NONE',  ( 0.000000000000000000, -1.000000000000000000, 0.000000000000000000 ) ) ;
#12560 = CARTESIAN_POINT ( 'NONE',  ( 47.74827507625478518, 62.59948385550240602, 7.007379884777227730 ) ) ;
#12561 = CARTESIAN_POINT ( 'NONE',  ( 45.86712807150323812, 51.29948385550240175, -5.649768623646098220 ) ) ;
#12562 = CIRCLE ( 'NONE', #13207, 15.00000000000000000 ) ;
#12563 = EDGE_CURVE ( 'NONE', #2067, #12293, #4315, .T. ) ;
#12564 = ORIENTED_EDGE ( 'NONE', *, *, #2714, .F. ) ;
#12565 = VECTOR ( 'NONE', #994, 1000.000000000000000 ) ;
#12566 = ORIENTED_EDGE ( 'NONE', *, *, #9580, .F. ) ;
#12567 = CARTESIAN_POINT ( 'NONE',  ( 15.00000000000000178, -20.00000000000000000, -50.00000000000000000 ) ) ;
#12568 = CARTESIAN_POINT ( 'NONE',  ( 0.000000000000000000, 0.000000000000000000, -4.974599999999998801 ) ) ;
#12569 = CIRCLE ( 'NONE', #617, 6.080745460913608902 ) ;
#12570 = DIRECTION ( 'NONE',  ( 0.000000000000000000, 0.000000000000000000, 1.000000000000000000 ) ) ;
#12571 = CARTESIAN_POINT ( 'NONE',  ( 49.97728705011488159, 45.49948385550240459, -7.000000000000000888 ) ) ;
#12572 = CARTESIAN_POINT ( 'NONE',  ( 56.65037692655921120, 49.10051614449766078, 2.184720259617097593 ) ) ;
#12573 = CARTESIAN_POINT ( 'NONE',  ( -2.499999999999999556, 3.061616997868382648E-16, 3.469446951953614189E-15 ) ) ;
#12574 = CARTESIAN_POINT ( 'NONE',  ( 55.96859303347804371, 46.19948385550238612, 4.306917132069425946 ) ) ;
#12575 = DIRECTION ( 'NONE',  ( 1.000000000000000000, -0.000000000000000000, -0.000000000000000000 ) ) ;
#12576 = CARTESIAN_POINT ( 'NONE',  ( 47.42335538002188144, 54.59948385550240602, 8.007379884777233059 ) ) ;
#12577 = AXIS2_PLACEMENT_3D ( 'NONE', #11328, #13182, #658 ) ;
#12578 = ORIENTED_EDGE ( 'NONE', *, *, #13172, .F. ) ;
#12579 = ORIENTED_EDGE ( 'NONE', *, *, #8305, .T. ) ;
#12580 = AXIS2_PLACEMENT_3D ( 'NONE', #8043, #10038, #13145 ) ;
#12581 = EDGE_CURVE ( 'NONE', #13574, #6658, #6232, .T. ) ;
#12582 = DIRECTION ( 'NONE',  ( 0.000000000000000000, 0.000000000000000000, -1.000000000000000000 ) ) ;
#12583 =( NAMED_UNIT ( * ) PLANE_ANGLE_UNIT ( ) SI_UNIT ( $, .RADIAN. ) );
#12584 = FACE_OUTER_BOUND ( 'NONE', #13112, .T. ) ;
#12585 = CARTESIAN_POINT ( 'NONE',  ( 6.371506350351447523, -5.409331239960139648, -0.8483282427581471108 ) ) ;
#12586 = LINE ( 'NONE', #5340, #6775 ) ;
#12587 = CARTESIAN_POINT ( 'NONE',  ( 55.11794222512599362, 46.80051614449766362, -3.688883143319583446 ) ) ;
#12588 = CARTESIAN_POINT ( 'NONE',  ( 54.09612160359792199, 61.30051614449766362, 5.676469297603124353 ) ) ;
#12589 = EDGE_CURVE ( 'NONE', #9920, #2907, #1210, .T. ) ;
#12590 = CARTESIAN_POINT ( 'NONE',  ( 52.57664461997821093, 63.40051614449765083, 8.007379884777206414 ) ) ;
#12591 = CARTESIAN_POINT ( 'NONE',  ( 4.000000000000000888, 1.563622288139206118, -0.2253451193528334950 ) ) ;
#12592 = CARTESIAN_POINT ( 'NONE',  ( 57.61547081786810764, 58.90051614449766504, -2.450534656007114176 ) ) ;
#12593 = EDGE_LOOP ( 'NONE', ( #2198, #1506, #5044, #9776, #4849 ) ) ;
#12594 = VERTEX_POINT ( 'NONE', #12007 ) ;
#12595 = ORIENTED_EDGE ( 'NONE', *, *, #13369, .T. ) ;
#12596 = AXIS2_PLACEMENT_3D ( 'NONE', #4927, #4854, #9139 ) ;
#12597 = EDGE_CURVE ( 'NONE', #7922, #12594, #9861, .T. ) ;
#12598 = DIRECTION ( 'NONE',  ( -0.04542589977017699732, 0.9989677110047501252, 0.000000000000000000 ) ) ;
#12599 = CARTESIAN_POINT ( 'NONE',  ( -30.00000000000000000, 4.999999999999989342, 0.000000000000000000 ) ) ;
#12600 = EDGE_CURVE ( 'NONE', #10838, #7994, #7851, .T. ) ;
#12601 = DIRECTION ( 'NONE',  ( -0.000000000000000000, -0.000000000000000000, 1.000000000000000000 ) ) ;
#12602 = FACE_OUTER_BOUND ( 'NONE', #10722, .T. ) ;
#12603 = EDGE_CURVE ( 'NONE', #690, #11255, #2284, .T. ) ;
#12604 = CARTESIAN_POINT ( 'NONE',  ( 56.30877334542961421, 49.99948385550240459, -0.02388180880520959434 ) ) ;
#12605 = CARTESIAN_POINT ( 'NONE',  ( 1.925929944387235853E-31, 15.00000000000001599, 9.999999999999998224 ) ) ;
#12606 = CARTESIAN_POINT ( 'NONE',  ( 45.27934281921082516, 45.70051614449766220, 6.458785618021089192 ) ) ;
#12607 = CARTESIAN_POINT ( 'NONE',  ( 4.000000000000000000, -2.309401076758514915, -3.433295621305383349 ) ) ;
#12608 = LINE ( 'NONE', #2937, #3016 ) ;
#12609 = CARTESIAN_POINT ( 'NONE',  ( 3.880206590543185730, 3.396506438958505125, -1.117078279489029935 ) ) ;
#12610 = CARTESIAN_POINT ( 'NONE',  ( 54.13287192849671214, 48.70051614449766220, -5.649768623646139964 ) ) ;
#12611 = CARTESIAN_POINT ( 'NONE',  ( 44.91013252490152752, 58.79948385550240175, 3.727524721679198461 ) ) ;
#12612 = DIRECTION ( 'NONE',  ( -1.000000000000000000, 0.000000000000000000, 0.000000000000000000 ) ) ;
#12613 = ORIENTED_EDGE ( 'NONE', *, *, #1226, .F. ) ;
#12614 = CARTESIAN_POINT ( 'NONE',  ( 2.649999999999988809, 15.00000000000001599, -15.00000000000000000 ) ) ;
#12615 = ORIENTED_EDGE ( 'NONE', *, *, #6676, .T. ) ;
#12616 = DIRECTION ( 'NONE',  ( 0.000000000000000000, 0.000000000000000000, -1.000000000000000000 ) ) ;
#12617 = CIRCLE ( 'NONE', #12822, 12.49999999999999645 ) ;
#12618 = PRODUCT_DEFINITION_SHAPE ( 'NONE', 'NONE',  #9454 ) ;
#12619 = CYLINDRICAL_SURFACE ( 'NONE', #117, 2.000000000000000888 ) ;
#12620 = CARTESIAN_POINT ( 'NONE',  ( 4.142654963991859951, 2.035398498734348305, -3.525413613457315076 ) ) ;
#12621 = ADVANCED_FACE ( 'NONE', ( #13030 ), #9636, .F. ) ;
#12622 = CARTESIAN_POINT ( 'NONE',  ( 52.25172492374522903, 53.59948385550241312, -7.007379884777225953 ) ) ;
#12623 = CARTESIAN_POINT ( 'NONE',  ( 0.1750025118121568690, 4.719839900820621104, -3.469254087858248070 ) ) ;
#12624 = CARTESIAN_POINT ( 'NONE',  ( 48.02776887271750184, 53.60051614449765367, 5.992620115222795363 ) ) ;
#12625 = CARTESIAN_POINT ( 'NONE',  ( 0.3126073911695746443, -2.020725942163797750, -3.499999999999999556 ) ) ;
#12626 = CARTESIAN_POINT ( 'NONE',  ( 43.33558569842703179, 65.09948385550239891, -2.141517661632099223 ) ) ;
#12627 = CARTESIAN_POINT ( 'NONE',  ( 56.65037692655918988, 63.89948385550239607, -2.184720259617163762 ) ) ;
#12628 = CARTESIAN_POINT ( 'NONE',  ( 43.34962307344081012, 56.89948385550240317, 2.184720259617164650 ) ) ;
#12629 = AXIS2_PLACEMENT_3D ( 'NONE', #6060, #11364, #10109 ) ;
#12630 = VECTOR ( 'NONE', #3561, 1000.000000000000000 ) ;
#12631 = EDGE_LOOP ( 'NONE', ( #8083, #2892 ) ) ;
#12632 = ORIENTED_EDGE ( 'NONE', *, *, #4161, .F. ) ;
#12633 = CARTESIAN_POINT ( 'NONE',  ( -2.742827927723112236, -3.035229711105190464, -3.433252694550595230 ) ) ;
#12634 = DIRECTION ( 'NONE',  ( 0.1305261922200524338, -0.9914448613738102711, 0.000000000000000000 ) ) ;
#12635 = CARTESIAN_POINT ( 'NONE',  ( 3.129923130707922496, -23.63917314727666152, -8.999999999999996447 ) ) ;
#12636 = VECTOR ( 'NONE', #499, 1000.000000000000000 ) ;
#12637 = CARTESIAN_POINT ( 'NONE',  ( 8.500000000000000000, 0.000000000000000000, 0.000000000000000000 ) ) ;
#12638 = FACE_OUTER_BOUND ( 'NONE', #10940, .T. ) ;
#12639 = CIRCLE ( 'NONE', #935, 15.00000000000000000 ) ;
#12640 = CARTESIAN_POINT ( 'NONE',  ( 47.74827507625469281, 50.40051614449764372, -7.007379884777203749 ) ) ;
#12641 = CARTESIAN_POINT ( 'NONE',  ( 62.49999999999998579, 32.50000000000001421, -15.00000000000000000 ) ) ;
#12642 = CARTESIAN_POINT ( 'NONE',  ( 56.65037692655918988, 47.89948385550240317, -2.184720259617163762 ) ) ;
#12643 = DIRECTION ( 'NONE',  ( 0.000000000000000000, 0.000000000000000000, -1.000000000000000000 ) ) ;
#12644 = CARTESIAN_POINT ( 'NONE',  ( 52.62207051974839089, 56.39948385550241028, 7.992620115222770494 ) ) ;
#12645 = ORIENTED_EDGE ( 'NONE', *, *, #12292, .F. ) ;
#12646 = ORIENTED_EDGE ( 'NONE', *, *, #4640, .T. ) ;
#12647 = CARTESIAN_POINT ( 'NONE',  ( 0.000000000000000000, 0.000000000000000000, 0.000000000000000000 ) ) ;
#12648 = DIRECTION ( 'NONE',  ( -1.000000000000000000, 0.000000000000000000, -0.000000000000000000 ) ) ;
#12649 = DIRECTION ( 'NONE',  ( 1.000000000000000000, 0.000000000000000000, 0.000000000000000000 ) ) ;
#12650 = CARTESIAN_POINT ( 'NONE',  ( 0.5636800770130377947, 4.293361309317166530, -3.531542292954102713 ) ) ;
#12651 = CARTESIAN_POINT ( 'NONE',  ( 49.97728705011494554, 49.50051614449766646, 6.000000000000000888 ) ) ;
#12652 = CARTESIAN_POINT ( 'NONE',  ( 44.03140696652198471, 57.80051614449766362, 4.306917132069485454 ) ) ;
#12653 = CARTESIAN_POINT ( 'NONE',  ( 47.37792948025162332, 49.39948385550241028, -7.992620115222770494 ) ) ;
#12654 = DIRECTION ( 'NONE',  ( -1.000000000000000000, -3.469446951953615175E-16, -0.000000000000000000 ) ) ;
#12655 = CARTESIAN_POINT ( 'NONE',  ( 52.57664461997821093, 59.40051614449765793, 8.007379884777206414 ) ) ;
#12656 = EDGE_CURVE ( 'NONE', #1406, #10456, #379, .T. ) ;
#12657 = ORIENTED_EDGE ( 'NONE', *, *, #5805, .T. ) ;
#12658 = VERTEX_POINT ( 'NONE', #4815 ) ;
#12659 = ORIENTED_EDGE ( 'NONE', *, *, #6225, .T. ) ;
#12660 = CARTESIAN_POINT ( 'NONE',  ( -6.259644161404860030E-16, -4.618802153517027165, -3.433295621305388234 ) ) ;
#12661 = CARTESIAN_POINT ( 'NONE',  ( -3.098410542199071749, -7.060458129626440815, 0.000000000000000000 ) ) ;
#12663 = AXIS2_PLACEMENT_3D ( 'NONE', #5503, #6542, #1053 ) ;
#12662 = LINE ( 'NONE', #7364, #4965 ) ;
#12664 = CARTESIAN_POINT ( 'NONE',  ( 0.000000000000000000, 3.755786496842903495E-16, 3.500000000000000000 ) ) ;
#12665 = CARTESIAN_POINT ( 'NONE',  ( 46.45491332379572924, 53.29948385550240886, -4.840751629271157874 ) ) ;
#12666 = CARTESIAN_POINT ( 'NONE',  ( 44.03140696652193498, 65.19948385550240744, -4.306917132069424170 ) ) ;
#12667 = CARTESIAN_POINT ( 'NONE',  ( 54.68390685589039890, 45.30051614449766362, 6.485486291978072693 ) ) ;
#12668 = DIRECTION ( 'NONE',  ( -0.000000000000000000, -0.000000000000000000, 1.000000000000000000 ) ) ;
#12669 = PLANE ( 'NONE',  #5374 ) ;
#12670 = DIRECTION ( 'NONE',  ( -1.000000000000000000, -0.000000000000000000, -0.000000000000000000 ) ) ;
#12671 = CARTESIAN_POINT ( 'NONE',  ( 45.86712807150329496, 59.70051614449766220, 5.649768623646139964 ) ) ;
#12672 = CARTESIAN_POINT ( 'NONE',  ( 56.30877334542961421, 57.99948385550241170, -0.02388180880520959434 ) ) ;
#12673 = DIRECTION ( 'NONE',  ( 0.000000000000000000, 0.000000000000000000, 1.000000000000000000 ) ) ;
#12674 = CIRCLE ( 'NONE', #1628, 15.00000000000000000 ) ;
#12675 = VERTEX_POINT ( 'NONE', #7997 ) ;
#12676 = DIRECTION ( 'NONE',  ( -1.000000000000000000, 0.000000000000000000, 0.000000000000000000 ) ) ;
#12677 = AXIS2_PLACEMENT_3D ( 'NONE', #2098, #11517, #12403 ) ;
#12678 = VERTEX_POINT ( 'NONE', #12208 ) ;
#12679 = CARTESIAN_POINT ( 'NONE',  ( 0.000000000000000000, 3.031088913245533423, -1.750000000000004885 ) ) ;
#12680 = CARTESIAN_POINT ( 'NONE',  ( 62.49999999999998579, 40.00000000000001421, -9.999999999999998224 ) ) ;
#12681 = AXIS2_PLACEMENT_3D ( 'NONE', #57, #12701, #1688 ) ;
#12682 = EDGE_CURVE ( 'NONE', #12202, #5130, #7416, .T. ) ;
#12683 = CARTESIAN_POINT ( 'NONE',  ( -4.000000000000000000, -1.942223658245633811, -0.3516579909967644246 ) ) ;
#12684 = CARTESIAN_POINT ( 'NONE',  ( 57.36023556966787851, 51.99948385550238328, -0.02388180880522424582 ) ) ;
#12685 = VECTOR ( 'NONE', #6979, 1000.000000000000000 ) ;
#12686 = CARTESIAN_POINT ( 'NONE',  ( -4.236525694536558362, 2.416953475386465211, -3.751298745799836354 ) ) ;
#12687 = CARTESIAN_POINT ( 'NONE',  ( 56.30877334542961421, 55.00051614449766646, 0.02388180880515774693 ) ) ;
#12688 = CARTESIAN_POINT ( 'NONE',  ( 1.925929944387235853E-31, 15.00000000000001599, -9.999999999999998224 ) ) ;
#12689 = VECTOR ( 'NONE', #3781, 1000.000000000000000 ) ;
#12690 = CARTESIAN_POINT ( 'NONE',  ( 44.03140696652192787, 63.19948385550240744, -4.306917132069425058 ) ) ;
#12691 = DIRECTION ( 'NONE',  ( -0.000000000000000000, -0.000000000000000000, 1.000000000000000000 ) ) ;
#12692 = CARTESIAN_POINT ( 'NONE',  ( 43.34962307344081012, 62.89948385550241028, 2.184720259617164650 ) ) ;
#12693 = ORIENTED_EDGE ( 'NONE', *, *, #5704, .T. ) ;
#12694 = EDGE_CURVE ( 'NONE', #6155, #3730, #10016, .T. ) ;
#12695 = EDGE_CURVE ( 'NONE', #278, #7167, #2965, .T. ) ;
#12696 = EDGE_LOOP ( 'NONE', ( #13061, #9341, #2625, #7810 ) ) ;
#12697 = AXIS2_PLACEMENT_3D ( 'NONE', #2735, #1684, #5927 ) ;
#12698 = FACE_OUTER_BOUND ( 'NONE', #4991, .T. ) ;
#12699 = DIRECTION ( 'NONE',  ( 0.000000000000000000, -1.224646799147353207E-16, 1.000000000000000000 ) ) ;
#12700 = CARTESIAN_POINT ( 'NONE',  ( -2.345747346278108214, 3.264484291692489215, -0.01223254789873409049 ) ) ;
#12701 = DIRECTION ( 'NONE',  ( -1.000000000000000000, -0.000000000000000000, -0.000000000000000000 ) ) ;
#12702 = CARTESIAN_POINT ( 'NONE',  ( 56.65037692655918988, 47.89948385550240317, -2.184720259617163762 ) ) ;
#12703 = CARTESIAN_POINT ( 'NONE',  ( 49.97728705011495265, 45.50051614449765935, 7.000000000000000888 ) ) ;
#12704 = DIRECTION ( 'NONE',  ( 0.000000000000000000, 1.000000000000000000, 0.000000000000000000 ) ) ;
#12705 = CARTESIAN_POINT ( 'NONE',  ( 47.42335538002188144, 64.59948385550241312, 8.007379884777233059 ) ) ;
#12706 = ADVANCED_FACE ( 'NONE', ( #2948 ), #11382, .F. ) ;
#12707 = CARTESIAN_POINT ( 'NONE',  ( 52.57664461997811856, 53.59948385550240602, -8.007379884777229506 ) ) ;
#12708 = ORIENTED_EDGE ( 'NONE', *, *, #9047, .F. ) ;
#12709 = VERTEX_POINT ( 'NONE', #3979 ) ;
#12710 = DIRECTION ( 'NONE',  ( -1.000000000000000000, -0.000000000000000000, -0.000000000000000000 ) ) ;
#12711 = AXIS2_PLACEMENT_3D ( 'NONE', #3834, #5852, #11015 ) ;
#12712 = AXIS2_PLACEMENT_3D ( 'NONE', #2101, #1049, #3149 ) ;
#12713 = EDGE_CURVE ( 'NONE', #12234, #6107, #9614, .T. ) ;
#12714 = DIRECTION ( 'NONE',  ( 0.000000000000000000, 1.000000000000000000, 0.000000000000000000 ) ) ;
#12715 = CARTESIAN_POINT ( 'NONE',  ( 3.129923130707922496, -23.63917314727666152, -8.999999999999996447 ) ) ;
#12716 = CARTESIAN_POINT ( 'NONE',  ( 48.02776887271750184, 45.60051614449765367, 5.992620115222795363 ) ) ;
#12717 = CARTESIAN_POINT ( 'NONE',  ( 57.36023556966787851, 61.00051614449765935, 0.02388180880515038476 ) ) ;
#12718 = CARTESIAN_POINT ( 'NONE',  ( 54.72065718078924590, 48.29948385550240175, 6.458785618021043895 ) ) ;
#12719 = DIRECTION ( 'NONE',  ( -0.6520673188974834833, 0.7581610723493047432, 1.805535875966851803E-17 ) ) ;
#12720 = CARTESIAN_POINT ( 'NONE',  ( 58.41169779390614281, 59.00051614449766646, 0.02388180880515032231 ) ) ;
#12721 = PRODUCT ( 'Mounting block', 'Mounting block', '', ( #6129 ) ) ;
#12722 = VERTEX_POINT ( 'NONE', #5102 ) ;
#12723 = ORIENTED_EDGE ( 'NONE', *, *, #770, .F. ) ;
#12724 = ORIENTED_EDGE ( 'NONE', *, *, #11996, .T. ) ;
#12725 = CARTESIAN_POINT ( 'NONE',  ( -2.000000000000007550, -3.464101615137749945, 0.000000000000000000 ) ) ;
#12726 = CARTESIAN_POINT ( 'NONE',  ( 6.403457969954085449, 2.888443235695447253, -5.002930439003170804 ) ) ;
#12727 = CARTESIAN_POINT ( 'NONE',  ( 3.973110223767137850, 2.263269463293572928E-11, 3.565797985667434222 ) ) ;
#12728 = DIRECTION ( 'NONE',  ( 1.000000000000000000, 0.000000000000000000, -0.000000000000000000 ) ) ;
#12729 = CARTESIAN_POINT ( 'NONE',  ( 51.92680522751233951, 49.59948385550241312, -6.007379884777223289 ) ) ;
#12730 = LINE ( 'NONE', #6402, #5745 ) ;
#12731 = CARTESIAN_POINT ( 'NONE',  ( 54.72065718078918906, 46.70051614449766220, -6.458785618021089192 ) ) ;
#12732 = CARTESIAN_POINT ( 'NONE',  ( 3.999999999999999112, -1.539600717839012978, -3.300726591567080703 ) ) ;
#12733 = DIRECTION ( 'NONE',  ( -1.000000000000000000, 0.000000000000000000, 0.000000000000000000 ) ) ;
#12734 = CARTESIAN_POINT ( 'NONE',  ( 52.29715082351538769, 54.60051614449766788, -6.992620115222796251 ) ) ;
#12735 = CARTESIAN_POINT ( 'NONE',  ( 49.97728705011488870, 59.49948385550240459, -6.000000000000000888 ) ) ;
#12736 = DIRECTION ( 'NONE',  ( -0.000000000000000000, 0.8660254037844387076, 0.5000000000000001110 ) ) ;
#12737 = ORIENTED_EDGE ( 'NONE', *, *, #9951, .F. ) ;
#12738 = DIRECTION ( 'NONE',  ( 0.000000000000000000, 0.000000000000000000, -1.000000000000000000 ) ) ;
#12739 = ORIENTED_EDGE ( 'NONE', *, *, #8052, .F. ) ;
#12740 = CARTESIAN_POINT ( 'NONE',  ( -5.686050877451574337, -5.768780236673276995, -1.000000000000000000 ) ) ;
#12741 = PLANE ( 'NONE',  #1846 ) ;
#12742 = DIRECTION ( 'NONE',  ( -0.7779254092217071648, -0.6283566325640553840, 0.000000000000000000 ) ) ;
#12743 = CARTESIAN_POINT ( 'NONE',  ( 49.97728705011488159, 53.49948385550240459, -7.000000000000000888 ) ) ;
#12744 = DIRECTION ( 'NONE',  ( 1.000000000000000000, 0.000000000000000000, 0.000000000000000000 ) ) ;
#12745 = CARTESIAN_POINT ( 'NONE',  ( 46.45491332379576477, 49.70051614449766220, 4.840751629271188961 ) ) ;
#12746 = EDGE_CURVE ( 'NONE', #4573, #9060, #11383, .T. ) ;
#12747 = LINE ( 'NONE', #1203, #9756 ) ;
#12748 = CARTESIAN_POINT ( 'NONE',  ( 2.059999999999998721, 0.000000000000000000, -0.3080913168122742518 ) ) ;
#12749 = CARTESIAN_POINT ( 'NONE',  ( 6.481779955677436256, -5.820445026626584806, 1.740800559574606662E-15 ) ) ;
#12750 = CARTESIAN_POINT ( 'NONE',  ( 54.09612160359786515, 61.69948385550240744, -5.676469297603166098 ) ) ;
#12751 = ADVANCED_BREP_SHAPE_REPRESENTATION ( '', ( #5785, #430 ), #10821 ) ;
#12752 = CARTESIAN_POINT ( 'NONE',  ( 1.000000000000002442, -20.00000000000000000, 8.999999999999998224 ) ) ;
#12753 = ORIENTED_EDGE ( 'NONE', *, *, #4811, .F. ) ;
#12754 = CIRCLE ( 'NONE', #5710, 5.000000000000000888 ) ;
#12755 = ORIENTED_EDGE ( 'NONE', *, *, #8643, .F. ) ;
#12756 = ORIENTED_EDGE ( 'NONE', *, *, #11744, .F. ) ;
#12757 = DIRECTION ( 'NONE',  ( -1.000000000000000000, 9.251858538542972814E-17, -0.000000000000000000 ) ) ;
#12758 = EDGE_CURVE ( 'NONE', #9009, #9556, #12481, .T. ) ;
#12759 = CARTESIAN_POINT ( 'NONE',  ( -14.99999999999999645, -20.00000000000005329, 9.000000000000000000 ) ) ;
#12760 = CARTESIAN_POINT ( 'NONE',  ( 3.880206590543186618, -3.396506438958517116, 1.117078279489015502 ) ) ;
#12761 = EDGE_CURVE ( 'NONE', #5149, #5888, #8272, .T. ) ;
#12762 = CARTESIAN_POINT ( 'NONE',  ( -74.99999999999997158, -39.99999999999998579, -10.00000000000000000 ) ) ;
#12763 = EDGE_CURVE ( 'NONE', #9523, #9424, #4054, .T. ) ;
#12764 = CARTESIAN_POINT ( 'NONE',  ( 55.96859303347805081, 50.19948385550240744, 4.306917132069425058 ) ) ;
#12765 = CARTESIAN_POINT ( 'NONE',  ( 43.34962307344078880, 46.10051614449766078, -2.184720259617096705 ) ) ;
#12766 = EDGE_CURVE ( 'NONE', #3637, #1915, #2040, .T. ) ;
#12767 = AXIS2_PLACEMENT_3D ( 'NONE', #6906, #4765, #13043 ) ;
#12768 = CARTESIAN_POINT ( 'NONE',  ( -0.9999999999999995559, -15.10102051443364246, 15.00000000000000355 ) ) ;
#12769 = CARTESIAN_POINT ( 'NONE',  ( 43.34962307344081012, 46.89948385550240317, 2.184720259617164650 ) ) ;
#12770 = DIRECTION ( 'NONE',  ( -1.000000000000000000, -0.000000000000000000, -0.000000000000000000 ) ) ;
#12771 = CARTESIAN_POINT ( 'NONE',  ( 45.31609314410967926, 54.69948385550240033, 6.485486291978119766 ) ) ;
#12772 = ORIENTED_EDGE ( 'NONE', *, *, #6862, .T. ) ;
#12773 = ORIENTED_EDGE ( 'NONE', *, *, #12109, .F. ) ;
#12774 = VECTOR ( 'NONE', #7642, 1000.000000000000000 ) ;
#12775 = CARTESIAN_POINT ( 'NONE',  ( -30.00000000000000000, -7.500000000000011546, 10.00000000000000000 ) ) ;
#12776 = AXIS2_PLACEMENT_3D ( 'NONE', #13153, #9230, #4739 ) ;
#12777 = CIRCLE ( 'NONE', #13212, 1.999999999999998224 ) ;
#12778 = CARTESIAN_POINT ( 'NONE',  ( 0.1217565302851095904, 2.351289329882149559, 2.927447417349536618 ) ) ;
#12779 = CARTESIAN_POINT ( 'NONE',  ( 50.02271294988506156, 50.50051614449765935, -6.000000000000000888 ) ) ;
#12780 = CARTESIAN_POINT ( 'NONE',  ( 49.97728705011495265, 61.50051614449765935, 7.000000000000000888 ) ) ;
#12781 = CARTESIAN_POINT ( 'NONE',  ( 56.79116909180259398, 63.20051614449766220, 4.963592699178938972 ) ) ;
#12782 = AXIS2_PLACEMENT_3D ( 'NONE', #2826, #9942, #10151 ) ;
#12783 = LINE ( 'NONE', #3462, #12850 ) ;
#12784 = CARTESIAN_POINT ( 'NONE',  ( 56.81924384183006538, 54.80051614449764941, -4.924951120819380357 ) ) ;
#12785 = ORIENTED_EDGE ( 'NONE', *, *, #8296, .F. ) ;
#12786 = ORIENTED_EDGE ( 'NONE', *, *, #1091, .F. ) ;
#12787 = ORIENTED_EDGE ( 'NONE', *, *, #2481, .T. ) ;
#12788 = ORIENTED_EDGE ( 'NONE', *, *, #6618, .F. ) ;
#12789 = CARTESIAN_POINT ( 'NONE',  ( 50.02271294988505446, 44.50051614449765935, -7.000000000000000888 ) ) ;
#12790 = CARTESIAN_POINT ( 'NONE',  ( 50.00000000000000000, 15.00000000000000000, -4.000000000000003553 ) ) ;
#12792 = AXIS2_PLACEMENT_3D ( 'NONE', #6566, #4550, #12016 ) ;
#12791 = FACE_OUTER_BOUND ( 'NONE', #8587, .T. ) ;
#12793 = LINE ( 'NONE', #10726, #9935 ) ;
#12794 = DIRECTION ( 'NONE',  ( -0.000000000000000000, -0.000000000000000000, 1.000000000000000000 ) ) ;
#12795 = ADVANCED_FACE ( 'NONE', ( #12411 ), #6309, .F. ) ;
#12796 = FILL_AREA_STYLE_COLOUR ( '', #2571 ) ;
#12797 = CARTESIAN_POINT ( 'NONE',  ( 53.50833635130540955, 47.69948385550240744, -4.867452303228209765 ) ) ;
#12798 = FACE_OUTER_BOUND ( 'NONE', #5718, .T. ) ;
#12799 = CARTESIAN_POINT ( 'NONE',  ( 43.18075615816994173, 45.80051614449766362, 4.924951120819380357 ) ) ;
#12800 = CARTESIAN_POINT ( 'NONE',  ( 10.00000000000000000, 15.00000000000001776, 15.00000000000000000 ) ) ;
#12801 = DIRECTION ( 'NONE',  ( -0.8660254037844377084, -0.5000000000000015543, 0.000000000000000000 ) ) ;
#12802 = CARTESIAN_POINT ( 'NONE',  ( 43.33558569842706021, 55.90051614449765793, 2.141517661632167169 ) ) ;
#12803 = CARTESIAN_POINT ( 'NONE',  ( 51.97223112728254790, 58.39948385550241028, 5.992620115222778487 ) ) ;
#12804 = VECTOR ( 'NONE', #1161, 1000.000000000000000 ) ;
#12805 = VERTEX_POINT ( 'NONE', #10272 ) ;
#12806 = CARTESIAN_POINT ( 'NONE',  ( 2.000000000000000000, 1.773042676681340524, -2.059984127722458425E-15 ) ) ;
#12807 = ORIENTED_EDGE ( 'NONE', *, *, #1798, .F. ) ;
#12808 = CARTESIAN_POINT ( 'NONE',  ( 30.00000000000000000, 7.500000000000011546, 10.00000000000000000 ) ) ;
#12809 = CARTESIAN_POINT ( 'NONE',  ( 9.999999999999994671, 20.00000000000001421, 15.00000000000000000 ) ) ;
#12810 = CARTESIAN_POINT ( 'NONE',  ( 4.165266963751723672, 2.049631966911992009, -3.550066703508905963 ) ) ;
#12811 = CARTESIAN_POINT ( 'NONE',  ( 50.02271294988512551, 50.49948385550240459, 7.000000000000000888 ) ) ;
#12812 = AXIS2_PLACEMENT_3D ( 'NONE', #396, #2405, #12978 ) ;
#12813 = DIRECTION ( 'NONE',  ( 0.000000000000000000, 0.000000000000000000, 1.000000000000000000 ) ) ;
#12814 = CARTESIAN_POINT ( 'NONE',  ( 51.97223112728249816, 52.60051614449765367, -5.992620115222793586 ) ) ;
#12815 = CYLINDRICAL_SURFACE ( 'NONE', #6252, 5.000000000000000888 ) ;
#12816 = CARTESIAN_POINT ( 'NONE',  ( 4.000000000000000000, 0.000000000000000000, 0.000000000000000000 ) ) ;
#12817 = FILL_AREA_STYLE ('',( #10691 ) ) ;
#12818 = CARTESIAN_POINT ( 'NONE',  ( 44.05948171654949874, 60.79948385550240886, 4.345558710429105354 ) ) ;
#12819 = CARTESIAN_POINT ( 'NONE',  ( 0.8816464618332836567, -24.71833652004169934, 9.000000000000000000 ) ) ;
#12820 = B_SPLINE_CURVE_WITH_KNOTS ( 'NONE', 3,
 ( #12725, #2491, #3333, #4435, #282, #6659 ),
 .UNSPECIFIED., .F., .F.,
 ( 4, 2, 4 ),
 ( 0.002365888236228001588, 0.003551327329835089319, 0.004736766423442177049 ),
 .UNSPECIFIED. ) ;
#12821 = ORIENTED_EDGE ( 'NONE', *, *, #8983, .T. ) ;
#12822 = AXIS2_PLACEMENT_3D ( 'NONE', #8071, #2737, #12343 ) ;
#12823 = UNCERTAINTY_MEASURE_WITH_UNIT (LENGTH_MEASURE( 1.000000000000000082E-05 ), #7576, 'distance_accuracy_value', 'NONE');
#12824 = ORIENTED_EDGE ( 'NONE', *, *, #10743, .F. ) ;
#12825 = ORIENTED_EDGE ( 'NONE', *, *, #6654, .T. ) ;
#12826 = CARTESIAN_POINT ( 'NONE',  ( -1.274258131565027874, -3.883108878240886241, -3.220599429844051009 ) ) ;
#12827 = EDGE_CURVE ( 'NONE', #3147, #9171, #7244, .T. ) ;
#12828 = CARTESIAN_POINT ( 'NONE',  ( -0.1481481481481481122, -4.797713218419819903, 0.000000000000000000 ) ) ;
#12829 = CARTESIAN_POINT ( 'NONE',  ( 4.200000000000001954, 0.000000000000000000, -2.200000000000001066 ) ) ;
#12830 = CARTESIAN_POINT ( 'NONE',  ( 2.000000000000000000, 0.000000000000000000, 0.000000000000000000 ) ) ;
#12831 = CARTESIAN_POINT ( 'NONE',  ( 54.13287192849676188, 50.29948385550240175, 5.649768623646098220 ) ) ;
#12832 = AXIS2_PLACEMENT_3D ( 'NONE', #1885, #13351, #12193 ) ;
#12833 = CARTESIAN_POINT ( 'NONE',  ( 49.97728705011495265, 55.50051614449766646, 7.000000000000000888 ) ) ;
#12834 = CARTESIAN_POINT ( 'NONE',  ( 55.48859070151218020, 45.00000000000002132, -4.999999999999993783 ) ) ;
#12835 = AXIS2_PLACEMENT_3D ( 'NONE', #2569, #2500, #5558 ) ;
#12836 = CIRCLE ( 'NONE', #13274, 4.799999999999999822 ) ;
#12837 = CARTESIAN_POINT ( 'NONE',  ( 56.66441430157296821, 50.09948385550240602, 2.141517661632100111 ) ) ;
#12838 = SURFACE_STYLE_USAGE ( .BOTH. , #4416 ) ;
#12839 = CARTESIAN_POINT ( 'NONE',  ( 47.37792948025162332, 53.39948385550241028, -7.992620115222770494 ) ) ;
#12840 = VERTEX_POINT ( 'NONE', #784 ) ;
#12841 = ORIENTED_EDGE ( 'NONE', *, *, #6676, .F. ) ;
#12842 = AXIS2_PLACEMENT_3D ( 'NONE', #6948, #6064, #3762 ) ;
#12843 = CARTESIAN_POINT ( 'NONE',  ( 3.951447005078451813, 3.704664227300101143, 0.5833333333333334814 ) ) ;
#12844 = LINE ( 'NONE', #3455, #3332 ) ;
#12845 = CARTESIAN_POINT ( 'NONE',  ( 46.45491332379576477, 57.70051614449766930, 4.840751629271188961 ) ) ;
#12846 = CARTESIAN_POINT ( 'NONE',  ( 55.94051828345054389, 63.20051614449764799, 4.345558710429044957 ) ) ;
#12847 = CARTESIAN_POINT ( 'NONE',  ( 45.27934281921075410, 49.29948385550240886, -6.458785618021043895 ) ) ;
#12848 = DIRECTION ( 'NONE',  ( 1.000000000000000000, 0.000000000000000000, 0.000000000000000000 ) ) ;
#12849 = CARTESIAN_POINT ( 'NONE',  ( 57.60143344285435774, 57.10051614449766788, 2.493737253992045044 ) ) ;
#12850 = VECTOR ( 'NONE', #12719, 999.9999999999998863 ) ;
#12851 = ORIENTED_EDGE ( 'NONE', *, *, #12600, .F. ) ;
#12852 = EDGE_CURVE ( 'NONE', #8791, #12805, #1757, .T. ) ;
#12853 = ORIENTED_EDGE ( 'NONE', *, *, #10424, .T. ) ;
#12854 = ADVANCED_FACE ( 'NONE', ( #6288 ), #8514, .T. ) ;
#12855 = ORIENTED_EDGE ( 'NONE', *, *, #5768, .T. ) ;
#12856 = EDGE_LOOP ( 'NONE', ( #10039, #11269, #8975 ) ) ;
#12857 = FACE_OUTER_BOUND ( 'NONE', #9728, .T. ) ;
#12858 = CARTESIAN_POINT ( 'NONE',  ( 2.449293598294706513E-15, -20.00000000000000000, 15.00000000000000355 ) ) ;
#12859 = EDGE_CURVE ( 'NONE', #1843, #2996, #4986, .T. ) ;
#12860 = DIRECTION ( 'NONE',  ( 0.000000000000000000, 0.000000000000000000, -1.000000000000000000 ) ) ;
#12861 = LINE ( 'NONE', #8936, #461 ) ;
#12862 = CARTESIAN_POINT ( 'NONE',  ( 0.000000000000000000, 4.163799117101000559E-16, -3.299999999999999822 ) ) ;
#12863 = CARTESIAN_POINT ( 'NONE',  ( 50.02271294988511841, 52.49948385550241170, 6.000000000000000888 ) ) ;
#12864 = CARTESIAN_POINT ( 'NONE',  ( 43.34962307344078880, 46.10051614449766078, -2.184720259617096705 ) ) ;
#12865 = CARTESIAN_POINT ( 'NONE',  ( 58.41169779390614281, 49.00051614449765935, 0.02388180880515032231 ) ) ;
#12866 = FACE_OUTER_BOUND ( 'NONE', #550, .T. ) ;
#12867 = PLANE ( 'NONE',  #7132 ) ;
#12868 = CARTESIAN_POINT ( 'NONE',  ( 45.90387839640208512, 58.30051614449766362, -5.676469297603124353 ) ) ;
#12869 = CARTESIAN_POINT ( 'NONE',  ( 43.69122665457040000, 62.99948385550241170, 0.02388180880521036456 ) ) ;
#12870 = EDGE_LOOP ( 'NONE', ( #5825, #12041, #1486, #13313 ) ) ;
#12871 = DIRECTION ( 'NONE',  ( -1.000000000000000000, 0.000000000000000000, 0.000000000000000000 ) ) ;
#12872 = ORIENTED_EDGE ( 'NONE', *, *, #13336, .T. ) ;
#12873 = CARTESIAN_POINT ( 'NONE',  ( 6.367873360227555679, -2.886751345948119774, 4.999999999999999112 ) ) ;
#12874 = CARTESIAN_POINT ( 'NONE',  ( -31.74999999999995737, 0.000000000000000000, 0.000000000000000000 ) ) ;
#12875 = CARTESIAN_POINT ( 'NONE',  ( 3.880206590543187950, -2.665671387532591474, -2.382921720510934538 ) ) ;
#12876 = SHAPE_REPRESENTATION_RELATIONSHIP ( 'NONE' , 'NONE' ,  #7264, #9629 ) ;
#12877 = CARTESIAN_POINT ( 'NONE',  ( 49.97728705011488159, 51.49948385550240459, -7.000000000000000888 ) ) ;
#12878 = ADVANCED_FACE ( 'NONE', ( #10544, #236 ), #12741, .F. ) ;
#12879 = CARTESIAN_POINT ( 'NONE',  ( 20.00000000000000000, -20.00000000000000000, -23.00000000000000000 ) ) ;
#12880 = CARTESIAN_POINT ( 'NONE',  ( 46.45491332379576477, 55.70051614449766220, 4.840751629271188961 ) ) ;
#12881 = TOROIDAL_SURFACE ( 'NONE', #11585, 3.299999999999999822, 0.2000000000000000111 ) ;
#12882 = CYLINDRICAL_SURFACE ( 'NONE', #3353, 5.000000000000000888 ) ;
#12883 = DIRECTION ( 'NONE',  ( 0.000000000000000000, 1.000000000000000000, -1.345283343056720273E-15 ) ) ;
#12884 = DIRECTION ( 'NONE',  ( 0.000000000000000000, 0.000000000000000000, -1.000000000000000000 ) ) ;
#12885 = CARTESIAN_POINT ( 'NONE',  ( 42.63976443033212860, 56.99948385550241170, 0.02388180880522514787 ) ) ;
#12886 = DIRECTION ( 'NONE',  ( -0.000000000000000000, -1.000000000000000000, -0.000000000000000000 ) ) ;
#12887 = VERTEX_POINT ( 'NONE', #12680 ) ;
#12888 = CIRCLE ( 'NONE', #10253, 3.500000000000000000 ) ;
#12889 = CIRCLE ( 'NONE', #2749, 7.900000000000002132 ) ;
#12890 = ADVANCED_FACE ( 'NONE', ( #10614 ), #7444, .F. ) ;
#12891 = ORIENTED_EDGE ( 'NONE', *, *, #13384, .F. ) ;
#12892 = CARTESIAN_POINT ( 'NONE',  ( 4.082498951862917558, 4.041451884327382338, 3.558567857214853949E-17 ) ) ;
#12893 = CIRCLE ( 'NONE', #8058, 5.000000000000000888 ) ;
#12894 = CARTESIAN_POINT ( 'NONE',  ( 10.00000000000000000, 20.00000000000001421, 15.00000000000000000 ) ) ;
#12895 = FACE_OUTER_BOUND ( 'NONE', #4502, .T. ) ;
#12896 = DIRECTION ( 'NONE',  ( -0.000000000000000000, -0.000000000000000000, 1.000000000000000000 ) ) ;
#12897 = CARTESIAN_POINT ( 'NONE',  ( -75.00000000000001421, -2.602085213965211904E-14, 0.000000000000000000 ) ) ;
#12898 = CARTESIAN_POINT ( 'NONE',  ( 52.25172492374522903, 53.59948385550241312, -7.007379884777227730 ) ) ;
#12899 = VECTOR ( 'NONE', #8910, 1000.000000000000000 ) ;
#12900 = CARTESIAN_POINT ( 'NONE',  ( 55.96859303347802239, 56.80051614449764230, -4.306917132069484566 ) ) ;
#12901 = PLANE ( 'NONE',  #13449 ) ;
#12902 = CARTESIAN_POINT ( 'NONE',  ( 49.97728705011488159, 51.49948385550240459, -7.000000000000000888 ) ) ;
#12903 = CARTESIAN_POINT ( 'NONE',  ( -4.211140560182196957, -2.431303136016552013, -3.745885042887436178 ) ) ;
#12904 = PRODUCT_DEFINITION ( 'UNKNOWN', '', #1746, #2589 ) ;
#12905 = AXIS2_PLACEMENT_3D ( 'NONE', #5460, #316, #12699 ) ;
#12906 = CARTESIAN_POINT ( 'NONE',  ( 50.02271294988513972, 60.49948385550240459, 8.000000000000001776 ) ) ;
#12907 = ORIENTED_EDGE ( 'NONE', *, *, #5080, .F. ) ;
#12908 = ORIENTED_EDGE ( 'NONE', *, *, #1200, .F. ) ;
#12909 = ORIENTED_EDGE ( 'NONE', *, *, #12766, .F. ) ;
#12910 = CARTESIAN_POINT ( 'NONE',  ( 0.000000000000000000, 0.000000000000000000, 0.000000000000000000 ) ) ;
#12911 = DIRECTION ( 'NONE',  ( -0.000000000000000000, 1.000000000000000000, -0.000000000000000000 ) ) ;
#12912 = CARTESIAN_POINT ( 'NONE',  ( 53.54508667620424234, 52.70051614449766220, -4.840751629271188961 ) ) ;
#12913 = CARTESIAN_POINT ( 'NONE',  ( 6.534838248920896930, -2.951765777552406878, 5.112608298763836601 ) ) ;
#12914 = CARTESIAN_POINT ( 'NONE',  ( 52.57664461997811856, 53.59948385550240602, -8.007379884777229506 ) ) ;
#12915 = CARTESIAN_POINT ( 'NONE',  ( 45.86712807150323812, 59.29948385550240175, -5.649768623646098220 ) ) ;
#12916 = CARTESIAN_POINT ( 'NONE',  ( 4.175326769692858875, -4.121399112977860213, 3.677815466159040336E-14 ) ) ;
#12917 = EDGE_CURVE ( 'NONE', #7909, #5823, #3154, .T. ) ;
#12918 = CARTESIAN_POINT ( 'NONE',  ( 57.61547081786812896, 46.09948385550240602, 2.450534656007040901 ) ) ;
#12919 = VERTEX_POINT ( 'NONE', #2370 ) ;
#12920 = VERTEX_POINT ( 'NONE', #4191 ) ;
#12921 = ORIENTED_EDGE ( 'NONE', *, *, #11790, .F. ) ;
#12922 = VERTEX_POINT ( 'NONE', #8414 ) ;
#12923 = CARTESIAN_POINT ( 'NONE',  ( 1.925929944387235853E-31, 15.00000000000001599, 15.00000000000000000 ) ) ;
#12924 = ADVANCED_FACE ( 'NONE', ( #36 ), #12619, .T. ) ;
#12925 = CARTESIAN_POINT ( 'NONE',  ( -65.14999999999996305, 32.50000000000001421, 10.00000000000000000 ) ) ;
#12926 = PLANE ( 'NONE',  #11630 ) ;
#12927 = CARTESIAN_POINT ( 'NONE',  ( 53.50833635130540955, 55.69948385550240744, -4.867452303228209765 ) ) ;
#12928 = CARTESIAN_POINT ( 'NONE',  ( 45.90387839640208512, 48.30051614449765651, -5.676469297603124353 ) ) ;
#12929 = EDGE_CURVE ( 'NONE', #10387, #4812, #10895, .T. ) ;
#12930 = CARTESIAN_POINT ( 'NONE',  ( 47.42335538002180328, 54.40051614449765793, -8.007379884777206414 ) ) ;
#12931 = VECTOR ( 'NONE', #24, 1000.000000000000000 ) ;
#12932 = EDGE_CURVE ( 'NONE', #1735, #10124, #2061, .T. ) ;
#12933 = DIRECTION ( 'NONE',  ( 0.3420201433256622736, 1.150791560227853228E-16, 0.9396926207859106484 ) ) ;
#12934 = FACE_OUTER_BOUND ( 'NONE', #9790, .T. ) ;
#12935 = AXIS2_PLACEMENT_3D ( 'NONE', #10728, #411, #2286 ) ;
#12936 = CARTESIAN_POINT ( 'NONE',  ( 56.66441430157294690, 56.90051614449766504, -2.141517661632166281 ) ) ;
#12937 = ORIENTED_EDGE ( 'NONE', *, *, #12447, .F. ) ;
#12938 = CARTESIAN_POINT ( 'NONE',  ( 0.000000000000000000, 4.041451884327382338, 0.000000000000000000 ) ) ;
#12939 = ORIENTED_EDGE ( 'NONE', *, *, #2542, .T. ) ;
#12940 = CARTESIAN_POINT ( 'NONE',  ( 0.4465819873852002742, 2.886751345948125547, 4.999999999999999112 ) ) ;
#12941 = CARTESIAN_POINT ( 'NONE',  ( 4.078421086530217288, -3.990950201428958621, -1.000000000000000000 ) ) ;
#12942 = DIRECTION ( 'NONE',  ( -1.000000000000000000, 0.000000000000000000, 0.000000000000000000 ) ) ;
#12943 = CARTESIAN_POINT ( 'NONE',  ( 50.02271294988512551, 56.49948385550240459, 7.000000000000000888 ) ) ;
#12944 = ADVANCED_FACE ( 'NONE', ( #7574 ), #11350, .T. ) ;
#12945 = EDGE_CURVE ( 'NONE', #8787, #9119, #9511, .T. ) ;
#12946 = FACE_OUTER_BOUND ( 'NONE', #11180, .T. ) ;
#12947 = CARTESIAN_POINT ( 'NONE',  ( 53.50833635130544508, 57.30051614449767072, 4.867452303228181343 ) ) ;
#12948 = CARTESIAN_POINT ( 'NONE',  ( 2.449293598294706513E-15, -20.00000000000000000, 15.00000000000000355 ) ) ;
#12949 = CARTESIAN_POINT ( 'NONE',  ( 0.000000000000000000, 0.000000000000000000, 0.000000000000000000 ) ) ;
#12950 = CARTESIAN_POINT ( 'NONE',  ( 50.02271294988511841, 46.49948385550240459, 6.000000000000000888 ) ) ;
#12951 = CARTESIAN_POINT ( 'NONE',  ( 4.024499207728657879, -2.323545700935587988, -3.572172305156509964 ) ) ;
#12952 = EDGE_LOOP ( 'NONE', ( #798, #3671, #10053 ) ) ;
#12953 = EDGE_LOOP ( 'NONE', ( #7844, #10625, #12564, #2959 ) ) ;
#12954 = UNCERTAINTY_MEASURE_WITH_UNIT (LENGTH_MEASURE( 1.000000000000000082E-05 ), #6354, 'distance_accuracy_value', 'NONE');
#12955 = ORIENTED_EDGE ( 'NONE', *, *, #689, .F. ) ;
#12956 = CARTESIAN_POINT ( 'NONE',  ( 30.00000000000000000, 1.040834085586084888E-14, 0.000000000000000000 ) ) ;
#12957 = CARTESIAN_POINT ( 'NONE',  ( 4.000000000000000000, -2.309401076758516691, -0.4999999999999995559 ) ) ;
#12958 = CYLINDRICAL_SURFACE ( 'NONE', #5557, 5.000000000000000888 ) ;
#12959 = SHAPE_REPRESENTATION_RELATIONSHIP ( 'NONE' , 'NONE' ,  #10521, #11781 ) ;
#12960 = DIRECTION ( 'NONE',  ( -3.469446951953614682E-16, 1.000000000000000000, 0.000000000000000000 ) ) ;
#12961 = CARTESIAN_POINT ( 'NONE',  ( 4.101954839143060028, 2.368264730582927857, -3.681130640444267854 ) ) ;
#12962 = CARTESIAN_POINT ( 'NONE',  ( 44.03140696652193498, 53.19948385550240033, -4.306917132069424170 ) ) ;
#12963 = EDGE_CURVE ( 'NONE', #720, #4149, #726, .T. ) ;
#12964 = CARTESIAN_POINT ( 'NONE',  ( 57.36023556966787851, 55.00051614449765225, 0.02388180880515038476 ) ) ;
#12965 = EDGE_CURVE ( 'NONE', #5207, #4030, #10806, .T. ) ;
#12966 = DIRECTION ( 'NONE',  ( -9.858538378746663627E-23, 5.031452844637890958E-23, -1.000000000000000000 ) ) ;
#12967 = CARTESIAN_POINT ( 'NONE',  ( 43.34962307344081012, 52.89948385550240317, 2.184720259617164650 ) ) ;
#12968 = CARTESIAN_POINT ( 'NONE',  ( 43.34962307344081012, 48.89948385550240317, 2.184720259617164650 ) ) ;
#12969 = VECTOR ( 'NONE', #10233, 1000.000000000000000 ) ;
#12970 = CARTESIAN_POINT ( 'NONE',  ( 47.42335538002188144, 64.59948385550241312, 8.007379884777233059 ) ) ;
#12971 = VERTEX_POINT ( 'NONE', #4454 ) ;
#12972 = ORIENTED_EDGE ( 'NONE', *, *, #12603, .F. ) ;
#12973 = CYLINDRICAL_SURFACE ( 'NONE', #13641, 1.999999999999998224 ) ;
#12974 = EDGE_LOOP ( 'NONE', ( #8918, #10356, #13279, #9305 ) ) ;
#12975 = DIRECTION ( 'NONE',  ( 1.000000000000000000, 0.000000000000000000, -0.000000000000000000 ) ) ;
#12976 = APPLICATION_CONTEXT ( 'automotive_design' ) ;
#12977 = AXIS2_PLACEMENT_3D ( 'NONE', #9795, #3574, #1407 ) ;
#12978 = DIRECTION ( 'NONE',  ( 1.000000000000000000, 0.000000000000000000, 0.000000000000000000 ) ) ;
#12979 = AXIS2_PLACEMENT_3D ( 'NONE', #8094, #12299, #2831 ) ;
#12980 = CARTESIAN_POINT ( 'NONE',  ( 55.69932041026405045, 53.10051614449767499, 1.875703265242156359 ) ) ;
#12981 = CARTESIAN_POINT ( 'NONE',  ( 2.000000000000000000, 1.773042676681340524, -2.059984127722458425E-15 ) ) ;
#12982 = CARTESIAN_POINT ( 'NONE',  ( 41.58830220609386430, 50.99948385550241170, 0.02388180880523263147 ) ) ;
#12983 = CARTESIAN_POINT ( 'NONE',  ( 56.65037692655918988, 53.89948385550240317, -2.184720259617163762 ) ) ;
#12984 = LINE ( 'NONE', #7754, #11102 ) ;
#12985 = CARTESIAN_POINT ( 'NONE',  ( 56.79116909180259398, 61.20051614449766220, 4.963592699178938972 ) ) ;
#12986 = B_SPLINE_CURVE_WITH_KNOTS ( 'NONE', 3,
 ( #1112, #6535, #11774, #7566, #90, #2359, #1244, #9770 ),
 .UNSPECIFIED., .F., .F.,
 ( 4, 2, 2, 4 ),
 ( 0.002921158011986707288, 0.003648658599403064012, 0.004376159186819420302, 0.005831160361652131148 ),
 .UNSPECIFIED. ) ;
#12987 = AXIS2_PLACEMENT_3D ( 'NONE', #9206, #10302, #10575 ) ;
#12989 = EDGE_CURVE ( 'NONE', #2854, #9289, #10682, .T. ) ;
#12988 = ORIENTED_EDGE ( 'NONE', *, *, #5441, .T. ) ;
#12990 = VECTOR ( 'NONE', #4602, 1000.000000000000000 ) ;
#12991 = ORIENTED_EDGE ( 'NONE', *, *, #5591, .F. ) ;
#12992 = ORIENTED_EDGE ( 'NONE', *, *, #2013, .F. ) ;
#12993 = ORIENTED_EDGE ( 'NONE', *, *, #2977, .T. ) ;
#12994 = DIRECTION ( 'NONE',  ( -1.000000000000000000, 0.000000000000000000, 0.000000000000000000 ) ) ;
#12995 = FACE_OUTER_BOUND ( 'NONE', #4033, .T. ) ;
#12996 = MECHANICAL_DESIGN_GEOMETRIC_PRESENTATION_REPRESENTATION (  '', ( #9269 ), #11466 ) ;
#12997 = CYLINDRICAL_SURFACE ( 'NONE', #12935, 15.00000000000000000 ) ;
#12998 = CARTESIAN_POINT ( 'NONE',  ( 44.28664221472220675, 59.09948385550240602, -1.832500667257165317 ) ) ;
#12999 = CARTESIAN_POINT ( 'NONE',  ( 55.96859303347802239, 46.80051614449766362, -4.306917132069484566 ) ) ;
#13000 = CARTESIAN_POINT ( 'NONE',  ( 45.27934281921082516, 55.70051614449766220, 6.458785618021089192 ) ) ;
#13001 = CARTESIAN_POINT ( 'NONE',  ( 4.000000000000000000, 2.309401076758515803, -0.4999999999999995559 ) ) ;
#13002 = DIRECTION ( 'NONE',  ( 1.000000000000000000, 0.000000000000000000, 0.000000000000000000 ) ) ;
#13003 = CARTESIAN_POINT ( 'NONE',  ( 56.66441430157294690, 62.90051614449765083, -2.141517661632166281 ) ) ;
#13004 = ORIENTED_EDGE ( 'NONE', *, *, #3208, .F. ) ;
#13005 = AXIS2_PLACEMENT_3D ( 'NONE', #367, #4873, #2580 ) ;
#13006 = AXIS2_PLACEMENT_3D ( 'NONE', #5475, #5744, #10844 ) ;
#13007 = CYLINDRICAL_SURFACE ( 'NONE', #6830, 8.099999999999999645 ) ;
#13008 = EDGE_CURVE ( 'NONE', #11823, #8572, #5243, .T. ) ;
#13009 = VERTEX_POINT ( 'NONE', #11782 ) ;
#13010 = FACE_OUTER_BOUND ( 'NONE', #13144, .T. ) ;
#13011 = ADVANCED_FACE ( 'NONE', ( #4385 ), #8610, .F. ) ;
#13012 = CARTESIAN_POINT ( 'NONE',  ( 75.00000000000001421, -7.499999999999971578, -10.00000000000000000 ) ) ;
#13013 = FACE_OUTER_BOUND ( 'NONE', #2489, .T. ) ;
#13014 = CARTESIAN_POINT ( 'NONE',  ( 0.000000000000000000, 0.000000000000000000, 0.000000000000000000 ) ) ;
#13015 = CARTESIAN_POINT ( 'NONE',  ( 57.36023556966787851, 55.99948385550239038, -0.02388180880522424582 ) ) ;
#13016 = MECHANICAL_DESIGN_GEOMETRIC_PRESENTATION_REPRESENTATION (  '', ( #648 ), #8416 ) ;
#13017 = VECTOR ( 'NONE', #4130, 1000.000000000000114 ) ;
#13018 = CARTESIAN_POINT ( 'NONE',  ( 44.91013252490150620, 56.20051614449766220, -3.727524721679154940 ) ) ;
#13019 = CARTESIAN_POINT ( 'NONE',  ( 4.170895651974849905, -2.054890354522598273, 3.559174498016383748 ) ) ;
#13020 = CARTESIAN_POINT ( 'NONE',  ( 6.534838248920899595, 5.903531555104835071, 8.098083288904839678E-18 ) ) ;
#13021 = CARTESIAN_POINT ( 'NONE',  ( 55.96859303347802239, 46.80051614449767072, -4.306917132069484566 ) ) ;
#13022 = CARTESIAN_POINT ( 'NONE',  ( 43.33558569842703179, 63.09948385550240602, -2.141517661632099223 ) ) ;
#13023 = FACE_OUTER_BOUND ( 'NONE', #6459, .T. ) ;
#13024 = VERTEX_POINT ( 'NONE', #9711 ) ;
#13025 = VERTEX_POINT ( 'NONE', #8681 ) ;
#13026 = VERTEX_POINT ( 'NONE', #3421 ) ;
#13027 = LINE ( 'NONE', #9028, #10112 ) ;
#13028 = EDGE_CURVE ( 'NONE', #4029, #5480, #83, .T. ) ;
#13029 = AXIS2_PLACEMENT_3D ( 'NONE', #7899, #10172, #5065 ) ;
#13030 = FACE_OUTER_BOUND ( 'NONE', #13224, .T. ) ;
#13031 = DIRECTION ( 'NONE',  ( -0.000000000000000000, -0.000000000000000000, -1.000000000000000000 ) ) ;
#13032 = DIRECTION ( 'NONE',  ( 0.000000000000000000, 1.000000000000000000, 0.000000000000000000 ) ) ;
#13033 = EDGE_CURVE ( 'NONE', #13009, #12154, #8927, .T. ) ;
#13034 = CARTESIAN_POINT ( 'NONE',  ( 4.142654963991859063, -2.035398498734348305, 3.525413613457315076 ) ) ;
#13035 = CARTESIAN_POINT ( 'NONE',  ( 49.97728705011495265, 53.50051614449765935, 7.000000000000000888 ) ) ;
#13036 = DIRECTION ( 'NONE',  ( 1.000000000000000000, 0.000000000000000000, 0.000000000000000000 ) ) ;
#13037 = CARTESIAN_POINT ( 'NONE',  ( 57.36023556966787851, 51.99948385550238328, -0.02388180880522424582 ) ) ;
#13038 = DIRECTION ( 'NONE',  ( 0.000000000000000000, 1.000000000000000000, 0.000000000000000000 ) ) ;
#13039 = CIRCLE ( 'NONE', #4907, 15.00000000000000000 ) ;
#13040 = CARTESIAN_POINT ( 'NONE',  ( 56.79116909180255135, 63.79948385550241596, -4.963592699179005585 ) ) ;
#13041 = VERTEX_POINT ( 'NONE', #12941 ) ;
#13042 = VERTEX_POINT ( 'NONE', #9779 ) ;
#13043 = DIRECTION ( 'NONE',  ( 0.000000000000000000, 0.000000000000000000, 1.000000000000000000 ) ) ;
#13044 = ORIENTED_EDGE ( 'NONE', *, *, #260, .F. ) ;
#13045 = CARTESIAN_POINT ( 'NONE',  ( -1.498123826657861368, -34.92499999999999716, -9.000000000000000000 ) ) ;
#13046 = AXIS2_PLACEMENT_3D ( 'NONE', #554, #5844, #8120 ) ;
#13047 = AXIS2_PLACEMENT_3D ( 'NONE', #3545, #3617, #1243 ) ;
#13048 = CARTESIAN_POINT ( 'NONE',  ( 0.000000000000000000, 3.031088913245533867, 1.750000000000002887 ) ) ;
#13049 = CARTESIAN_POINT ( 'NONE',  ( 53.50833635130544508, 55.30051614449765651, 4.867452303228181343 ) ) ;
#13050 = CARTESIAN_POINT ( 'NONE',  ( 0.02993401039713891598, -3.373851915354620257, -1.156317065392238774 ) ) ;
#13051 = CARTESIAN_POINT ( 'NONE',  ( 58.41169779390614281, 53.99948385550241170, -0.02388180880523160798 ) ) ;
#13052 = CARTESIAN_POINT ( 'NONE',  ( 44.05948171654949874, 54.79948385550241596, 4.345558710429105354 ) ) ;
#13053 = CARTESIAN_POINT ( 'NONE',  ( -14.14213562373094746, -25.00000000000000000, -50.00000000000000000 ) ) ;
#13054 = CARTESIAN_POINT ( 'NONE',  ( 43.20883090819742023, 64.20051614449766930, -4.963592699178938972 ) ) ;
#13055 = CIRCLE ( 'NONE', #9107, 12.49999999999999645 ) ;
#13056 = PRODUCT_DEFINITION_SHAPE ( 'NONE', 'NONE',  #13664 ) ;
#13057 = VECTOR ( 'NONE', #5990, 1000.000000000000000 ) ;
#13058 = ORIENTED_EDGE ( 'NONE', *, *, #12597, .F. ) ;
#13059 = ITEM_DEFINED_TRANSFORMATION ( 'NONE', 'NONE', #626,  #430 ) ;
#13060 = EDGE_LOOP ( 'NONE', ( #11420, #11908, #8660, #3468 ) ) ;
#13061 = ORIENTED_EDGE ( 'NONE', *, *, #7162, .T. ) ;
#13062 = VERTEX_POINT ( 'NONE', #11078 ) ;
#13063 = CARTESIAN_POINT ( 'NONE',  ( 2.449293598294706513E-15, -20.00000000000000000, 9.000000000000000000 ) ) ;
#13064 = DIRECTION ( 'NONE',  ( -0.000000000000000000, 0.000000000000000000, -1.000000000000000000 ) ) ;
#13065 =( NAMED_UNIT ( * ) SI_UNIT ( $, .STERADIAN. ) SOLID_ANGLE_UNIT ( ) );
#13066 = DIRECTION ( 'NONE',  ( -0.000000000000000000, -0.000000000000000000, 1.000000000000000000 ) ) ;
#13067 = CYLINDRICAL_SURFACE ( 'NONE', #9570, 2.649999999999985700 ) ;
#13068 = VECTOR ( 'NONE', #13099, 1000.000000000000000 ) ;
#13069 = CARTESIAN_POINT ( 'NONE',  ( 53.54508667620428497, 54.29948385550241596, 4.840751629271157874 ) ) ;
#13070 = CARTESIAN_POINT ( 'NONE',  ( 50.02271294988505446, 52.50051614449766646, -8.000000000000001776 ) ) ;
#13071 = AXIS2_PLACEMENT_3D ( 'NONE', #610, #13273, #12251 ) ;
#13072 = EDGE_CURVE ( 'NONE', #1878, #1542, #6509, .T. ) ;
#13073 = DIRECTION ( 'NONE',  ( -0.000000000000000000, -0.000000000000000000, -1.000000000000000000 ) ) ;
#13074 = LINE ( 'NONE', #6932, #12421 ) ;
#13075 = CARTESIAN_POINT ( 'NONE',  ( 54.72065718078918906, 44.70051614449765509, -6.458785618021089192 ) ) ;
#13076 = EDGE_LOOP ( 'NONE', ( #9287, #12339, #4885 ) ) ;
#13077 = CARTESIAN_POINT ( 'NONE',  ( 6.367873360227558344, -2.886751345948133984, -5.000000000000000000 ) ) ;
#13078 = ORIENTED_EDGE ( 'NONE', *, *, #883, .T. ) ;
#13079 = AXIS2_PLACEMENT_3D ( 'NONE', #7722, #244, #6687 ) ;
#13080 = DIRECTION ( 'NONE',  ( 0.000000000000000000, 0.000000000000000000, 1.000000000000000000 ) ) ;
#13081 = CARTESIAN_POINT ( 'NONE',  ( 6.092439126518621073, 1.005559546149547678, 4.999999999999999112 ) ) ;
#13082 = DIRECTION ( 'NONE',  ( -9.858538378746663627E-23, 5.031452844637890958E-23, -1.000000000000000000 ) ) ;
#13083 = CARTESIAN_POINT ( 'NONE',  ( 47.74827507625478518, 60.59948385550239891, 7.007379884777227730 ) ) ;
#13084 = CLOSED_SHELL ( 'NONE', ( #2217, #1080, #4952, #2675, #7939, #10907, #266, #10244, #8409, #6569, #3801, #9657, #2052, #7667, #4148, #10832, #7647, #6855, #5663, #8509, #1195, #10970, #13469, #12096, #94, #157, #1022, #8928, #960, #97, #3567, #1618, #4469, #5528, #3488, #4498, #7478, #6716 ) ) ;
#13085 = CARTESIAN_POINT ( 'NONE',  ( 50.02271294988506156, 60.50051614449766646, -6.000000000000000888 ) ) ;
#13086 = CARTESIAN_POINT ( 'NONE',  ( 13.61000000000001009, 0.000000000000000000, 2.000000000000001332 ) ) ;
#13087 = DIRECTION ( 'NONE',  ( 0.000000000000000000, -0.000000000000000000, 1.000000000000000000 ) ) ;
#13088 = CARTESIAN_POINT ( 'NONE',  ( 48.07319477248762496, 62.40051614449765793, -6.007379884777208190 ) ) ;
#13089 = CARTESIAN_POINT ( 'NONE',  ( 44.88205777487398507, 47.19948385550240744, -3.688883143319540814 ) ) ;
#13090 = LINE ( 'NONE', #13361, #11124 ) ;
#13091 = EDGE_LOOP ( 'NONE', ( #12613, #5058, #12615, #5615 ) ) ;
#13092 = UNCERTAINTY_MEASURE_WITH_UNIT (LENGTH_MEASURE( 1.000000000000000082E-05 ), #10859, 'distance_accuracy_value', 'NONE');
#13093 = EDGE_CURVE ( 'NONE', #10489, #12919, #7978, .T. ) ;
#13094 = ORIENTED_EDGE ( 'NONE', *, *, #4677, .T. ) ;
#13095 = FACE_OUTER_BOUND ( 'NONE', #5633, .T. ) ;
#13096 = CARTESIAN_POINT ( 'NONE',  ( 2.171643655288379993, -3.365003104552334978, -1.195831703456429434E-14 ) ) ;
#13097 = DIRECTION ( 'NONE',  ( 0.000000000000000000, -1.000000000000000000, 0.000000000000000000 ) ) ;
#13098 =( NAMED_UNIT ( * ) SI_UNIT ( $, .STERADIAN. ) SOLID_ANGLE_UNIT ( ) );
#13099 = DIRECTION ( 'NONE',  ( 0.000000000000000000, -1.000000000000000000, 9.783878858594328898E-16 ) ) ;
#13100 = DIRECTION ( 'NONE',  ( -1.000000000000000000, 0.000000000000000000, 0.000000000000000000 ) ) ;
#13101 = ADVANCED_FACE ( 'NONE', ( #4732 ), #2717, .T. ) ;
#13102 = AXIS2_PLACEMENT_3D ( 'NONE', #925, #3222, #1192 ) ;
#13103 = CARTESIAN_POINT ( 'NONE',  ( 44.03140696652198471, 53.80051614449766362, 4.306917132069485454 ) ) ;
#13104 = CARTESIAN_POINT ( 'NONE',  ( 6.204471256525345702, -0.9979289516723606202, -5.000000000000889955 ) ) ;
#13105 = CARTESIAN_POINT ( 'NONE',  ( 62.49999999999998579, 5.000000000000018652, 5.000000000000000000 ) ) ;
#13106 = CARTESIAN_POINT ( 'NONE',  ( 56.66441430157296821, 52.09948385550240602, 2.141517661632100111 ) ) ;
#13107 = ADVANCED_FACE ( 'NONE', ( #7779 ), #1185, .T. ) ;
#13108 = CARTESIAN_POINT ( 'NONE',  ( -74.99999999999997158, 20.00000000000001421, 15.00000000000000000 ) ) ;
#13109 = EDGE_CURVE ( 'NONE', #7271, #2163, #8949, .T. ) ;
#13110 = CARTESIAN_POINT ( 'NONE',  ( 47.42335538002188144, 60.59948385550240602, 8.007379884777233059 ) ) ;
#13111 = VECTOR ( 'NONE', #2648, 1000.000000000000000 ) ;
#13112 = EDGE_LOOP ( 'NONE', ( #10611, #11949, #31, #823, #8257, #4938, #7110, #2659, #346, #12853, #3026, #10571 ) ) ;
#13113 = ORIENTED_EDGE ( 'NONE', *, *, #10359, .F. ) ;
#13114 = LINE ( 'NONE', #3588, #3054 ) ;
#13115 = ORIENTED_EDGE ( 'NONE', *, *, #4935, .T. ) ;
#13116 = DIRECTION ( 'NONE',  ( 0.000000000000000000, 0.000000000000000000, -1.000000000000000000 ) ) ;
#13117 = AXIS2_PLACEMENT_3D ( 'NONE', #8896, #3295, #2245 ) ;
#13118 = CIRCLE ( 'NONE', #312, 12.50000000000000000 ) ;
#13119 = DIRECTION ( 'NONE',  ( 0.1836763462126260738, -0.9829867750086873635, -1.521953536530129477E-22 ) ) ;
#13120 = CARTESIAN_POINT ( 'NONE',  ( 44.91013252490150620, 52.20051614449766220, -3.727524721679154940 ) ) ;
#13121 = LINE ( 'NONE', #3458, #9045 ) ;
#13122 = CIRCLE ( 'NONE', #1199, 2.149999999999999023 ) ;
#13123 = CARTESIAN_POINT ( 'NONE',  ( 47.37792948025162332, 51.39948385550241028, -7.992620115222770494 ) ) ;
#13124 = CARTESIAN_POINT ( 'NONE',  ( 50.02271294988512551, 56.49948385550240459, 7.000000000000000888 ) ) ;
#13125 = CARTESIAN_POINT ( 'NONE',  ( 4.104070371397483541, -4.047367226856742661, 3.293285021600925981E-16 ) ) ;
#13126 = CARTESIAN_POINT ( 'NONE',  ( 56.81924384183011512, 46.19948385550240744, 4.924951120819313743 ) ) ;
#13127 = ORIENTED_EDGE ( 'NONE', *, *, #4163, .T. ) ;
#13128 = ORIENTED_EDGE ( 'NONE', *, *, #4202, .T. ) ;
#13129 = ORIENTED_EDGE ( 'NONE', *, *, #426, .T. ) ;
#13130 = ORIENTED_EDGE ( 'NONE', *, *, #12827, .F. ) ;
#13131 = ADVANCED_FACE ( 'NONE', ( #8810 ), #2508, .F. ) ;
#13132 = VECTOR ( 'NONE', #5375, 1000.000000000000000 ) ;
#13133 = CARTESIAN_POINT ( 'NONE',  ( -30.00000000000000000, -1.040834085586084257E-14, 0.000000000000000000 ) ) ;
#13134 = CARTESIAN_POINT ( 'NONE',  ( 20.00000000000000000, -14.99999999999999289, -23.00000000000000000 ) ) ;
#13135 = LINE ( 'NONE', #351, #4878 ) ;
#13136 = B_SPLINE_CURVE_WITH_KNOTS ( 'NONE', 3,
 ( #3192, #4361, #12916, #7421, #6387, #2142, #10585, #5680, #3725, #6780, #4842, #8926, #13125, #4708, #4637, #13253 ),
 .UNSPECIFIED., .F., .F.,
 ( 4, 3, 3, 3, 3, 4 ),
 ( -2.111273352579798197E-06, 0.000000000000000000, 3.519286887794736512E-05, 7.191842652068568460E-05, 0.0001049868727093669315, 0.0001382836236822145742 ),
 .UNSPECIFIED. ) ;
#13137 = CARTESIAN_POINT ( 'NONE',  ( 44.88205777487398507, 57.19948385550241454, -3.688883143319540814 ) ) ;
#13138 = CARTESIAN_POINT ( 'NONE',  ( 52.29715082351539479, 48.60051614449766078, -6.992620115222796251 ) ) ;
#13139 = CARTESIAN_POINT ( 'NONE',  ( 52.57664461997821093, 51.40051614449767214, 8.007379884777206414 ) ) ;
#13140 = CYLINDRICAL_SURFACE ( 'NONE', #907, 6.080745460913608902 ) ;
#13141 = CARTESIAN_POINT ( 'NONE',  ( 54.23491683972284960, 45.00000000000001421, -4.999999999999999112 ) ) ;
#13142 = CARTESIAN_POINT ( 'NONE',  ( 52.62207051974829852, 46.60051614449764656, -7.992620115222797139 ) ) ;
#13143 = PRODUCT_DEFINITION_SHAPE ( 'NONE', 'NONE',  #11897 ) ;
#13144 = EDGE_LOOP ( 'NONE', ( #10784, #2620, #7620, #507, #8710, #4746, #10230 ) ) ;
#13145 = DIRECTION ( 'NONE',  ( -1.000000000000000000, 0.000000000000000000, 0.000000000000000000 ) ) ;
#13146 = VERTEX_POINT ( 'NONE', #5775 ) ;
#13147 = CARTESIAN_POINT ( 'NONE',  ( -74.99999999999997158, -39.99999999999998579, 10.00000000000000000 ) ) ;
#13148 = CIRCLE ( 'NONE', #7217, 0.5999999999999980904 ) ;
#13149 = CARTESIAN_POINT ( 'NONE',  ( 2.385244779468109755E-15, -20.00000000000000000, -9.999999999999994671 ) ) ;
#13150 = CARTESIAN_POINT ( 'NONE',  ( 55.94051828345050836, 57.79948385550238754, -4.345558710429104465 ) ) ;
#13151 = CARTESIAN_POINT ( 'NONE',  ( 46.49166364869456913, 56.30051614449766362, -4.867452303228181343 ) ) ;
#13152 = CARTESIAN_POINT ( 'NONE',  ( 1.000000000000000000, -14.00000000000000000, 8.999999999999998224 ) ) ;
#13153 = CARTESIAN_POINT ( 'NONE',  ( 2.449293598294706513E-15, -20.00000000000000000, -50.00000000000000000 ) ) ;
#13154 = CARTESIAN_POINT ( 'NONE',  ( 45.86712807150329496, 47.70051614449766220, 5.649768623646139964 ) ) ;
#13155 = CARTESIAN_POINT ( 'NONE',  ( 44.03140696652192787, 63.19948385550240744, -4.306917132069425058 ) ) ;
#13156 = CARTESIAN_POINT ( 'NONE',  ( 0.000000000000000000, 0.000000000000000000, 0.000000000000000000 ) ) ;
#13157 = B_SPLINE_CURVE_WITH_KNOTS ( 'NONE', 3,
 ( #5830, #11133, #9210, #1653, #8105 ),
 .UNSPECIFIED., .F., .F.,
 ( 4, 1, 4 ),
 ( 5.640274452250024914E-20, 0.002309401076758505356, 0.004618802153517010713 ),
 .UNSPECIFIED. ) ;
#13158 = ORIENTED_EDGE ( 'NONE', *, *, #12531, .T. ) ;
#13159 = EDGE_LOOP ( 'NONE', ( #13058, #6015, #3533, #7881 ) ) ;
#13160 = DIRECTION ( 'NONE',  ( 0.000000000000000000, 0.000000000000000000, -1.000000000000000000 ) ) ;
#13161 = DIRECTION ( 'NONE',  ( 0.000000000000000000, 0.000000000000000000, -1.000000000000000000 ) ) ;
#13162 = DIRECTION ( 'NONE',  ( 0.000000000000000000, 0.000000000000000000, -1.000000000000000000 ) ) ;
#13163 = CARTESIAN_POINT ( 'NONE',  ( 2.000000000000000000, 0.8865213383406680414, -1.535500000000000975 ) ) ;
#13164 = CARTESIAN_POINT ( 'NONE',  ( 62.49999999999998579, 32.50000000000001421, 15.00000000000000000 ) ) ;
#13165 = EDGE_CURVE ( 'NONE', #1754, #9622, #3756, .T. ) ;
#13166 = CARTESIAN_POINT ( 'NONE',  ( 47.70284917648459100, 59.60051614449765367, 6.992620115222796251 ) ) ;
#13167 = CARTESIAN_POINT ( 'NONE',  ( 6.362366615495708366, 2.018765416950190961, -5.108861542006171597 ) ) ;
#13168 = LINE ( 'NONE', #7934, #5859 ) ;
#13169 = CARTESIAN_POINT ( 'NONE',  ( 49.97728705011488159, 55.49948385550240459, -7.000000000000000888 ) ) ;
#13170 = CARTESIAN_POINT ( 'NONE',  ( 45.90387839640214196, 48.69948385550240744, 5.676469297603166098 ) ) ;
#13171 = CARTESIAN_POINT ( 'NONE',  ( 57.61547081786812896, 62.09948385550240602, 2.450534656007040901 ) ) ;
#13172 = EDGE_CURVE ( 'NONE', #8572, #12920, #6940, .T. ) ;
#13173 = VERTEX_POINT ( 'NONE', #3688 ) ;
#13174 = ORIENTED_EDGE ( 'NONE', *, *, #3217, .F. ) ;
#13175 = CARTESIAN_POINT ( 'NONE',  ( 4.086262841041386373, 2.102637316508698451, -3.499999999999999556 ) ) ;
#13176 = ORIENTED_EDGE ( 'NONE', *, *, #6787, .F. ) ;
#13177 = EDGE_CURVE ( 'NONE', #2163, #2436, #3631, .T. ) ;
#13178 = DIRECTION ( 'NONE',  ( -0.000000000000000000, 0.000000000000000000, -1.000000000000000000 ) ) ;
#13179 = EDGE_CURVE ( 'NONE', #4979, #10817, #12674, .T. ) ;
#13180 = CARTESIAN_POINT ( 'NONE',  ( 6.385552186430389021, -2.886751345948133984, -5.000000000000000000 ) ) ;
#13181 = CARTESIAN_POINT ( 'NONE',  ( 55.71335778527780036, 58.90051614449766504, -1.832500667257213056 ) ) ;
#13182 = DIRECTION ( 'NONE',  ( -0.000000000000000000, -0.000000000000000000, 1.000000000000000000 ) ) ;
#13183 = CARTESIAN_POINT ( 'NONE',  ( 52.62207051974839089, 52.39948385550241028, 7.992620115222770494 ) ) ;
#13184 = CARTESIAN_POINT ( 'NONE',  ( 50.02271294988512551, 54.49948385550240459, 7.000000000000000888 ) ) ;
#13185 = DIRECTION ( 'NONE',  ( -1.000000000000000000, -0.000000000000000000, -0.000000000000000000 ) ) ;
#13186 = CARTESIAN_POINT ( 'NONE',  ( 47.42335538002180328, 62.40051614449765793, -8.007379884777206414 ) ) ;
#13187 = ORIENTED_EDGE ( 'NONE', *, *, #11527, .F. ) ;
#13188 = ITEM_DEFINED_TRANSFORMATION ( 'NONE', 'NONE', #214,  #430 ) ;
#13189 = ORIENTED_EDGE ( 'NONE', *, *, #11334, .T. ) ;
#13190 = VERTEX_POINT ( 'NONE', #7911 ) ;
#13191 = ORIENTED_EDGE ( 'NONE', *, *, #3665, .F. ) ;
#13192 = CARTESIAN_POINT ( 'NONE',  ( 45.15499999999999403, 0.000000000000000000, 2.500000000000000444 ) ) ;
#13193 = SHAPE_REPRESENTATION_RELATIONSHIP ( 'NONE' , 'NONE' ,  #3897, #1529 ) ;
#13194 = DIRECTION ( 'NONE',  ( 0.000000000000000000, 0.000000000000000000, -1.000000000000000000 ) ) ;
#13195 = FACE_OUTER_BOUND ( 'NONE', #11040, .T. ) ;
#13196 = CARTESIAN_POINT ( 'NONE',  ( 55.69932041026404335, 53.89948385550240317, -1.875703265242203432 ) ) ;
#13197 = CARTESIAN_POINT ( 'NONE',  ( 55.96859303347802239, 54.80051614449764941, -4.306917132069484566 ) ) ;
#13198 = CARTESIAN_POINT ( 'NONE',  ( 43.18075615816994173, 51.80051614449766362, 4.924951120819380357 ) ) ;
#13199 = CIRCLE ( 'NONE', #13653, 12.50000000000000000 ) ;
#13200 = DIRECTION ( 'NONE',  ( -0.000000000000000000, -0.000000000000000000, 1.000000000000000000 ) ) ;
#13201 = CARTESIAN_POINT ( 'NONE',  ( 56.81924384183006538, 44.80051614449766362, -4.924951120819380357 ) ) ;
#13202 =( GEOMETRIC_REPRESENTATION_CONTEXT ( 3 ) GLOBAL_UNCERTAINTY_ASSIGNED_CONTEXT ( ( #1472 ) ) GLOBAL_UNIT_ASSIGNED_CONTEXT ( ( #7653, #9722, #1397 ) ) REPRESENTATION_CONTEXT ( 'NONE', 'WORKASPACE' ) );
#13203 = ORIENTED_EDGE ( 'NONE', *, *, #1323, .F. ) ;
#13204 = CARTESIAN_POINT ( 'NONE',  ( -62.49999999999997158, 32.50000000000001421, 15.00000000000000000 ) ) ;
#13205 = ORIENTED_EDGE ( 'NONE', *, *, #7391, .F. ) ;
#13206 = EDGE_CURVE ( 'NONE', #12920, #10164, #8495, .T. ) ;
#13207 = AXIS2_PLACEMENT_3D ( 'NONE', #3083, #12616, #8477 ) ;
#13208 = CARTESIAN_POINT ( 'NONE',  ( 2.449293598294706513E-15, -20.00000000000000000, -50.00000000000000000 ) ) ;
#13209 = DIRECTION ( 'NONE',  ( 0.000000000000000000, -0.000000000000000000, 1.000000000000000000 ) ) ;
#13210 = DIRECTION ( 'NONE',  ( 1.000000000000000000, 0.000000000000000000, 0.000000000000000000 ) ) ;
#13211 = CARTESIAN_POINT ( 'NONE',  ( 43.34962307344081012, 56.89948385550240317, 2.184720259617164650 ) ) ;
#13212 = AXIS2_PLACEMENT_3D ( 'NONE', #10802, #6670, #9707 ) ;
#13213 = CARTESIAN_POINT ( 'NONE',  ( 43.34962307344081012, 50.89948385550241028, 2.184720259617164650 ) ) ;
#13214 = DIRECTION ( 'NONE',  ( 0.000000000000000000, 0.000000000000000000, 1.000000000000000000 ) ) ;
#13215 = DIRECTION ( 'NONE',  ( 0.000000000000000000, 0.000000000000000000, 1.000000000000000000 ) ) ;
#13216 = AXIS2_PLACEMENT_3D ( 'NONE', #11917, #5708, #12060 ) ;
#13217 = FACE_OUTER_BOUND ( 'NONE', #923, .T. ) ;
#13218 = CARTESIAN_POINT ( 'NONE',  ( 52.25172492374527877, 45.40051614449766504, 7.007379884777203749 ) ) ;
#13219 = CARTESIAN_POINT ( 'NONE',  ( 56.66441430157296821, 64.09948385550239891, 2.141517661632100111 ) ) ;
#13220 = CIRCLE ( 'NONE', #8605, 1.999999999999998224 ) ;
#13221 = DIRECTION ( 'NONE',  ( -0.000000000000000000, -0.000000000000000000, -1.000000000000000000 ) ) ;
#13222 = ORIENTED_EDGE ( 'NONE', *, *, #4180, .T. ) ;
#13223 = AXIS2_PLACEMENT_3D ( 'NONE', #2574, #2853, #10106 ) ;
#13224 = EDGE_LOOP ( 'NONE', ( #13589, #2925, #9116, #2002 ) ) ;
#13225 = ORIENTED_EDGE ( 'NONE', *, *, #360, .T. ) ;
#13226 = CARTESIAN_POINT ( 'NONE',  ( 22.00000000000000000, -20.00000000000000000, -20.00000000000000000 ) ) ;
#13227 = CARTESIAN_POINT ( 'NONE',  ( 2.000000000000005329, -3.464101615137751722, 0.000000000000000000 ) ) ;
#13228 = CARTESIAN_POINT ( 'NONE',  ( -13.49999999999999467, -20.00000000000005329, -9.000000000000000000 ) ) ;
#13229 = AXIS2_PLACEMENT_3D ( 'NONE', #385, #12966, #9668 ) ;
#13230 = SHAPE_REPRESENTATION_RELATIONSHIP ( 'NONE' , 'NONE' ,  #4503, #383 ) ;
#13231 = DIRECTION ( 'NONE',  ( 1.000000000000000000, 0.000000000000000000, -0.000000000000000000 ) ) ;
#13232 = DIRECTION ( 'NONE',  ( -1.000000000000000000, -0.000000000000000000, -0.000000000000000000 ) ) ;
#13233 = CARTESIAN_POINT ( 'NONE',  ( 43.33558569842706021, 57.90051614449766504, 2.141517661632167169 ) ) ;
#13234 = LINE ( 'NONE', #8352, #13017 ) ;
#13235 = CARTESIAN_POINT ( 'NONE',  ( -1.000000000000000000, -14.00000000000000000, -9.000000000000001776 ) ) ;
#13236 = CARTESIAN_POINT ( 'NONE',  ( 43.34962307344081012, 60.89948385550241028, 2.184720259617164650 ) ) ;
#13237 = CARTESIAN_POINT ( 'NONE',  ( 45.86712807150323812, 49.29948385550240175, -5.649768623646098220 ) ) ;
#13238 = EDGE_CURVE ( 'NONE', #2384, #4659, #5851, .T. ) ;
#13239 = CARTESIAN_POINT ( 'NONE',  ( 49.97728705011488159, 49.49948385550240459, -7.000000000000000888 ) ) ;
#13240 =( GEOMETRIC_REPRESENTATION_CONTEXT ( 3 ) GLOBAL_UNCERTAINTY_ASSIGNED_CONTEXT ( ( #1608 ) ) GLOBAL_UNIT_ASSIGNED_CONTEXT ( ( #10444, #3440, #3372 ) ) REPRESENTATION_CONTEXT ( 'NONE', 'WORKASPACE' ) );
#13241 = CIRCLE ( 'NONE', #11934, 0.4999999999999972244 ) ;
#13242 = EDGE_CURVE ( 'NONE', #1508, #7079, #1460, .T. ) ;
#13243 = ORIENTED_EDGE ( 'NONE', *, *, #6291, .F. ) ;
#13244 = ORIENTED_EDGE ( 'NONE', *, *, #13515, .F. ) ;
#13245 = VERTEX_POINT ( 'NONE', #9907 ) ;
#13246 = CARTESIAN_POINT ( 'NONE',  ( 30.00000000000000000, 1.040834085586084888E-14, 0.000000000000000000 ) ) ;
#13247 = DIRECTION ( 'NONE',  ( 0.000000000000000000, 0.000000000000000000, 1.000000000000000000 ) ) ;
#13248 = CARTESIAN_POINT ( 'NONE',  ( 44.30067958973594955, 64.10051614449766078, -1.875703265242155693 ) ) ;
#13249 = AXIS2_PLACEMENT_3D ( 'NONE', #6272, #5229, #9430 ) ;
#13250 = CARTESIAN_POINT ( 'NONE',  ( 6.367873360227558344, 5.773502691896261751, 0.000000000000000000 ) ) ;
#13251 = CARTESIAN_POINT ( 'NONE',  ( 49.97728705011486738, 57.49948385550241170, -8.000000000000001776 ) ) ;
#13252 = CARTESIAN_POINT ( 'NONE',  ( 43.34962307344081012, 64.89948385550239607, 2.184720259617164650 ) ) ;
#13253 = CARTESIAN_POINT ( 'NONE',  ( 4.071447262713890680, -4.041451884327386779, 0.000000000000000000 ) ) ;
#13254 = CARTESIAN_POINT ( 'NONE',  ( 42.38452918213188525, 53.09948385550240602, -2.450534656007040013 ) ) ;
#13255 = ORIENTED_EDGE ( 'NONE', *, *, #4540, .F. ) ;
#13256 = ITEM_DEFINED_TRANSFORMATION ( 'NONE', 'NONE', #7510,  #430 ) ;
#13257 = VECTOR ( 'NONE', #1615, 1000.000000000000114 ) ;
#13258 = ORIENTED_EDGE ( 'NONE', *, *, #1902, .T. ) ;
#13259 = VERTEX_POINT ( 'NONE', #4661 ) ;
#13260 = EDGE_LOOP ( 'NONE', ( #11762, #7621, #4048, #213 ) ) ;
#13261 = ADVANCED_FACE ( 'NONE', ( #8883 ), #4737, .T. ) ;
#13262 = CARTESIAN_POINT ( 'NONE',  ( 6.196878017913830305, -1.924500897298744961, 4.999999999999999112 ) ) ;
#13263 = DIRECTION ( 'NONE',  ( 1.000000000000000000, 0.000000000000000000, 0.000000000000000000 ) ) ;
#13264 = DIRECTION ( 'NONE',  ( 0.000000000000000000, 0.000000000000000000, -1.000000000000000000 ) ) ;
#13265 = CARTESIAN_POINT ( 'NONE',  ( 6.534838248920899595, -2.951765777552420644, -5.112608298763837489 ) ) ;
#13266 = CARTESIAN_POINT ( 'NONE',  ( -74.99999999999997158, 45.00000000000001421, 15.00000000000000000 ) ) ;
#13267 = CARTESIAN_POINT ( 'NONE',  ( 48.07319477248768180, 60.59948385550240602, 6.007379884777225953 ) ) ;
#13268 = CARTESIAN_POINT ( 'NONE',  ( 47.70284917648459810, 55.60051614449765367, 6.992620115222797139 ) ) ;
#13269 = CARTESIAN_POINT ( 'NONE',  ( 43.20883090819742023, 58.20051614449766220, -4.963592699178938972 ) ) ;
#13270 = AXIS2_PLACEMENT_3D ( 'NONE', #6942, #3893, #3757 ) ;
#13271 = CARTESIAN_POINT ( 'NONE',  ( 0.000000000000000000, 4.330127018922190096, -2.500000000000006217 ) ) ;
#13272 = AXIS2_PLACEMENT_3D ( 'NONE', #9769, #4515, #6797 ) ;
#13273 = DIRECTION ( 'NONE',  ( -9.710251638871371392E-17, -5.969973981896233748E-17, -1.000000000000000000 ) ) ;
#13274 = AXIS2_PLACEMENT_3D ( 'NONE', #12265, #11226, #10192 ) ;
#13275 = EDGE_CURVE ( 'NONE', #12511, #12971, #1855, .T. ) ;
#13276 = CARTESIAN_POINT ( 'NONE',  ( 44.05948171654945611, 62.20051614449764799, -4.345558710429044069 ) ) ;
#13277 = EDGE_CURVE ( 'NONE', #4104, #4218, #9597, .T. ) ;
#13279 = ORIENTED_EDGE ( 'NONE', *, *, #12472, .T. ) ;
#13278 = ORIENTED_EDGE ( 'NONE', *, *, #6031, .F. ) ;
#13280 = CARTESIAN_POINT ( 'NONE',  ( 0.000000000000000000, 0.5192545390863916310, -1.000000000000000000 ) ) ;
#13281 = EDGE_CURVE ( 'NONE', #9971, #5480, #3387, .T. ) ;
#13282 = ORIENTED_EDGE ( 'NONE', *, *, #2327, .T. ) ;
#13283 = AXIS2_PLACEMENT_3D ( 'NONE', #9276, #10093, #602 ) ;
#13284 = CARTESIAN_POINT ( 'NONE',  ( 53.50000000000000000, 0.000000000000000000, 0.000000000000000000 ) ) ;
#13285 = CYLINDRICAL_SURFACE ( 'NONE', #12629, 1.500000000000000666 ) ;
#13286 = CARTESIAN_POINT ( 'NONE',  ( 50.02271294988511841, 46.49948385550240459, 6.000000000000000888 ) ) ;
#13287 = CARTESIAN_POINT ( 'NONE',  ( 43.34962307344081012, 60.89948385550241028, 2.184720259617164650 ) ) ;
#13288 = DIRECTION ( 'NONE',  ( -1.000000000000000000, 0.000000000000000000, 1.224646799147353207E-16 ) ) ;
#13289 = DIRECTION ( 'NONE',  ( 1.000000000000000000, 0.000000000000000000, 0.000000000000000000 ) ) ;
#13290 = DIRECTION ( 'NONE',  ( -1.000000000000000000, -0.000000000000000000, -0.000000000000000000 ) ) ;
#13291 = CARTESIAN_POINT ( 'NONE',  ( 48.07319477248762496, 64.40051614449764372, -6.007379884777208190 ) ) ;
#13292 = CARTESIAN_POINT ( 'NONE',  ( 55.08986747509847248, 51.79948385550240175, -3.727524721679197572 ) ) ;
#13293 = CARTESIAN_POINT ( 'NONE',  ( 5.599999999999999645, 0.000000000000000000, 2.500000000000000444 ) ) ;
#13294 = EDGE_LOOP ( 'NONE', ( #12708, #10902, #6511, #6656 ) ) ;
#13295 = EDGE_LOOP ( 'NONE', ( #9674, #8880 ) ) ;
#13296 = ORIENTED_EDGE ( 'NONE', *, *, #4356, .T. ) ;
#13297 = DIRECTION ( 'NONE',  ( -0.000000000000000000, -0.000000000000000000, -1.000000000000000000 ) ) ;
#13298 = CARTESIAN_POINT ( 'NONE',  ( -62.49999999999997158, 32.50000000000001421, -15.00000000000000000 ) ) ;
#13299 = CARTESIAN_POINT ( 'NONE',  ( 6.436591462021362453, -2.894509378375957009, 5.013437306331779197 ) ) ;
#13300 =( LENGTH_UNIT ( ) NAMED_UNIT ( * ) SI_UNIT ( .MILLI., .METRE. ) );
#13301 = CARTESIAN_POINT ( 'NONE',  ( 1.000000000000000000, -14.00000000000000000, -9.000000000000001776 ) ) ;
#13302 = FACE_OUTER_BOUND ( 'NONE', #8347, .T. ) ;
#13303 = CARTESIAN_POINT ( 'NONE',  ( 54.09612160359792199, 59.30051614449766362, 5.676469297603124353 ) ) ;
#13304 = DIRECTION ( 'NONE',  ( -0.000000000000000000, -0.000000000000000000, 1.000000000000000000 ) ) ;
#13305 = CARTESIAN_POINT ( 'NONE',  ( 49.97728705011494554, 45.50051614449766646, 6.000000000000000888 ) ) ;
#13306 = DIRECTION ( 'NONE',  ( 0.000000000000000000, 0.000000000000000000, 1.000000000000000000 ) ) ;
#13307 = CARTESIAN_POINT ( 'NONE',  ( 49.97728705011488159, 61.49948385550240459, -7.000000000000000888 ) ) ;
#13308 = CARTESIAN_POINT ( 'NONE',  ( 43.34962307344081012, 52.89948385550240317, 2.184720259617164650 ) ) ;
#13309 = CARTESIAN_POINT ( 'NONE',  ( 43.33558569842703179, 51.09948385550240602, -2.141517661632099223 ) ) ;
#13310 = ORIENTED_EDGE ( 'NONE', *, *, #2139, .T. ) ;
#13311 = EDGE_LOOP ( 'NONE', ( #1681, #7169, #845, #7314 ) ) ;
#13312 = PLANE ( 'NONE',  #9462 ) ;
#13313 = ORIENTED_EDGE ( 'NONE', *, *, #6713, .F. ) ;
#13314 = DIRECTION ( 'NONE',  ( -1.000000000000000000, 0.000000000000000000, -0.000000000000000000 ) ) ;
#13315 = CARTESIAN_POINT ( 'NONE',  ( 0.8816464618332836567, -24.71833652004169934, 9.000000000000000000 ) ) ;
#13316 = CARTESIAN_POINT ( 'NONE',  ( 44.30067958973594955, 58.10051614449765367, -1.875703265242155693 ) ) ;
#13317 = CARTESIAN_POINT ( 'NONE',  ( 4.000000000000000000, 0.8378280264232961239, -3.220590601395640018 ) ) ;
#13318 = CARTESIAN_POINT ( 'NONE',  ( 54.68390685589033495, 59.69948385550240744, -6.485486291978119766 ) ) ;
#13319 = CARTESIAN_POINT ( 'NONE',  ( 57.36023556966787851, 63.99948385550241881, -0.02388180880522424582 ) ) ;
#13320 = LINE ( 'NONE', #8236, #490 ) ;
#13321 = CARTESIAN_POINT ( 'NONE',  ( 43.20883090819745576, 48.79948385550240175, 4.963592699179006473 ) ) ;
#13322 = EDGE_LOOP ( 'NONE', ( #146, #10453, #13464, #10002, #4777, #13479, #8583, #7483, #261, #1234, #1645, #8774, #3959, #3198, #7075, #11003, #6771, #5841, #6783, #7924, #6124, #821, #10051, #10407, #8115, #3081, #5753, #12336, #5514 ) ) ;
#13323 = CIRCLE ( 'NONE', #4744, 15.00000000000000000 ) ;
#13324 = CONTEXT_DEPENDENT_SHAPE_REPRESENTATION ( #4075, #34 ) ;
#13325 = EDGE_LOOP ( 'NONE', ( #7390, #3497, #3518, #10474 ) ) ;
#13326 = ORIENTED_EDGE ( 'NONE', *, *, #11678, .T. ) ;
#13327 = VERTEX_POINT ( 'NONE', #2930 ) ;
#13328 = VECTOR ( 'NONE', #6433, 1000.000000000000000 ) ;
#13329 = CARTESIAN_POINT ( 'NONE',  ( -2.804994570502171047, -3.229033611042465335, -3.526374918436838701 ) ) ;
#13330 = DIRECTION ( 'NONE',  ( -9.710251638871371392E-17, -5.969973981896233748E-17, -1.000000000000000000 ) ) ;
#13331 = CIRCLE ( 'NONE', #7406, 2.396904916527699214 ) ;
#13332 = CARTESIAN_POINT ( 'NONE',  ( 32.49999999999998579, 40.00000000000001421, 15.00000000000000000 ) ) ;
#13333 = DIRECTION ( 'NONE',  ( -1.000000000000000000, -0.000000000000000000, -0.000000000000000000 ) ) ;
#13334 = CARTESIAN_POINT ( 'NONE',  ( 55.11794222512601493, 60.19948385550240744, 3.688883143319541702 ) ) ;
#13335 = CARTESIAN_POINT ( 'NONE',  ( 42.63976443033212149, 56.00051614449765225, -0.02388180880514948964 ) ) ;
#13336 = EDGE_CURVE ( 'NONE', #6392, #3498, #10025, .T. ) ;
#13337 = AXIS2_PLACEMENT_3D ( 'NONE', #516, #6971, #8970 ) ;
#13338 = CARTESIAN_POINT ( 'NONE',  ( 50.02271294988505446, 56.50051614449767357, -8.000000000000001776 ) ) ;
#13339 = CYLINDRICAL_SURFACE ( 'NONE', #1814, 0.7500000000000000000 ) ;
#13340 = CARTESIAN_POINT ( 'NONE',  ( 54.72065718078918906, 52.70051614449766220, -6.458785618021089192 ) ) ;
#13342 = ORIENTED_EDGE ( 'NONE', *, *, #4584, .F. ) ;
#13341 = VERTEX_POINT ( 'NONE', #7080 ) ;
#13343 = AXIS2_PLACEMENT_3D ( 'NONE', #122, #4343, #8559 ) ;
#13344 = CARTESIAN_POINT ( 'NONE',  ( 1.654252653721905331, 3.663718938583014229, -0.01223254789873410957 ) ) ;
#13345 = VERTEX_POINT ( 'NONE', #693 ) ;
#13346 = EDGE_CURVE ( 'NONE', #8761, #13173, #9807, .T. ) ;
#13347 = ORIENTED_EDGE ( 'NONE', *, *, #8802, .F. ) ;
#13348 = EDGE_CURVE ( 'NONE', #2807, #6987, #6517, .T. ) ;
#13349 = EDGE_CURVE ( 'NONE', #5480, #6095, #3872, .T. ) ;
#13350 = CARTESIAN_POINT ( 'NONE',  ( 14.14213562373094923, -14.99999999999999112, -50.00000000000000000 ) ) ;
#13351 = DIRECTION ( 'NONE',  ( 0.000000000000000000, 0.000000000000000000, 1.000000000000000000 ) ) ;
#13352 = EDGE_CURVE ( 'NONE', #5185, #5079, #10392, .T. ) ;
#13353 = CARTESIAN_POINT ( 'NONE',  ( 55.08986747509847248, 45.79948385550240886, -3.727524721679197572 ) ) ;
#13354 = CARTESIAN_POINT ( 'NONE',  ( 42.63976443033212149, 56.99948385550241170, 0.02388180880522514787 ) ) ;
#13355 = B_SPLINE_CURVE_WITH_KNOTS ( 'NONE', 3,
 ( #10753, #9590, #4270, #4463, #8620, #8488 ),
 .UNSPECIFIED., .F., .F.,
 ( 4, 2, 4 ),
 ( 0.002044882221487525839, 0.003063384235218491979, 0.004081886248949458118 ),
 .UNSPECIFIED. ) ;
#13356 = CARTESIAN_POINT ( 'NONE',  ( 1.925929944387235853E-31, 15.00000000000001599, -9.999999999999998224 ) ) ;
#13357 = LINE ( 'NONE', #13152, #5134 ) ;
#13358 = CARTESIAN_POINT ( 'NONE',  ( 6.244297270355323448, 0.4917101305082447471, 5.105276777067912164 ) ) ;
#13359 = CARTESIAN_POINT ( 'NONE',  ( 45.86712807150329496, 51.70051614449766220, 5.649768623646139964 ) ) ;
#13360 = CARTESIAN_POINT ( 'NONE',  ( 43.69122665457040000, 50.99948385550241170, 0.02388180880521036456 ) ) ;
#13361 = CARTESIAN_POINT ( 'NONE',  ( -19.99999999999999289, -14.99999999999998579, -23.00000000000000000 ) ) ;
#13362 = ORIENTED_EDGE ( 'NONE', *, *, #3430, .T. ) ;
#13363 = ORIENTED_EDGE ( 'NONE', *, *, #10428, .F. ) ;
#13364 = ORIENTED_EDGE ( 'NONE', *, *, #2352, .T. ) ;
#13365 = CARTESIAN_POINT ( 'NONE',  ( 4.104070371397480876, -2.023683613428371775, -3.505122836902506922 ) ) ;
#13366 = VECTOR ( 'NONE', #6412, 1000.000000000000000 ) ;
#13367 = CARTESIAN_POINT ( 'NONE',  ( 45.60000000000000142, 2.516649172247811061E-16, -2.055000000000000160 ) ) ;
#13368 = CARTESIAN_POINT ( 'NONE',  ( 6.541171661047877173, -2.934678558896545386, -5.142480235691130552 ) ) ;
#13369 = EDGE_CURVE ( 'NONE', #6392, #4555, #9374, .T. ) ;
#13370 = CARTESIAN_POINT ( 'NONE',  ( 47.74827507625478518, 46.59948385550239891, 7.007379884777227730 ) ) ;
#13371 =( NAMED_UNIT ( * ) SI_UNIT ( $, .STERADIAN. ) SOLID_ANGLE_UNIT ( ) );
#13372 = CARTESIAN_POINT ( 'NONE',  ( 0.3108895250736384841, -2.416698868092693075, -5.000000000000000000 ) ) ;
#13373 = CARTESIAN_POINT ( 'NONE',  ( 53.54508667620424234, 46.70051614449766220, -4.840751629271188961 ) ) ;
#13374 = CARTESIAN_POINT ( 'NONE',  ( 0.000000000000000000, 20.00000000000001421, 9.999999999999998224 ) ) ;
#13375 = CARTESIAN_POINT ( 'NONE',  ( 50.02271294988512551, 60.49948385550240459, 7.000000000000000888 ) ) ;
#13376 = CARTESIAN_POINT ( 'NONE',  ( 52.25172492374522903, 53.59948385550241312, -7.007379884777225953 ) ) ;
#13377 = ORIENTED_EDGE ( 'NONE', *, *, #4599, .T. ) ;
#13378 = CARTESIAN_POINT ( 'NONE',  ( 44.03140696652192787, 47.19948385550240744, -4.306917132069425058 ) ) ;
#13379 = VERTEX_POINT ( 'NONE', #11289 ) ;
#13380 = ORIENTED_EDGE ( 'NONE', *, *, #995, .F. ) ;
#13381 = DIRECTION ( 'NONE',  ( -1.000000000000000000, 0.000000000000000000, 0.000000000000000000 ) ) ;
#13382 = VERTEX_POINT ( 'NONE', #9154 ) ;
#13383 = DIRECTION ( 'NONE',  ( 0.000000000000000000, 0.000000000000000000, -1.000000000000000000 ) ) ;
#13384 = EDGE_CURVE ( 'NONE', #8256, #1211, #95, .T. ) ;
#13385 = ADVANCED_FACE ( 'NONE', ( #9292 ), #3828, .F. ) ;
#13386 = DIRECTION ( 'NONE',  ( 0.000000000000000000, 0.000000000000000000, 1.000000000000000000 ) ) ;
#13387 = CARTESIAN_POINT ( 'NONE',  ( 6.436591462021357124, -2.894509378375969000, -5.013437306331776533 ) ) ;
#13388 = CARTESIAN_POINT ( 'NONE',  ( 43.69122665457040000, 62.00051614449766646, -0.02388180880515696977 ) ) ;
#13389 = CARTESIAN_POINT ( 'NONE',  ( -4.207491450040567571, 2.029819825146470524, -3.671670828759566074 ) ) ;
#13390 = CARTESIAN_POINT ( 'NONE',  ( 47.37792948025162332, 59.39948385550240317, -7.992620115222770494 ) ) ;
#13391 = CARTESIAN_POINT ( 'NONE',  ( 52.25172492374522903, 61.59948385550239891, -7.007379884777225953 ) ) ;
#13392 = CARTESIAN_POINT ( 'NONE',  ( 50.02271294988505446, 64.50051614449765225, -7.000000000000000888 ) ) ;
#13393 = CARTESIAN_POINT ( 'NONE',  ( 43.18075615816989199, 49.19948385550240744, -4.924951120819313743 ) ) ;
#13394 = ORIENTED_EDGE ( 'NONE', *, *, #4766, .T. ) ;
#13395 = ORIENTED_EDGE ( 'NONE', *, *, #9895, .T. ) ;
#13396 = EDGE_LOOP ( 'NONE', ( #4231, #12785, #9745, #7022 ) ) ;
#13397 = DIRECTION ( 'NONE',  ( 0.000000000000000000, 1.000000000000000000, 0.000000000000000000 ) ) ;
#13398 = DIRECTION ( 'NONE',  ( -1.000000000000000000, 0.000000000000000000, 0.000000000000000000 ) ) ;
#13399 = DIRECTION ( 'NONE',  ( 0.000000000000000000, 0.000000000000000000, -1.000000000000000000 ) ) ;
#13400 = CARTESIAN_POINT ( 'NONE',  ( 0.000000000000000000, 0.000000000000000000, 0.000000000000000000 ) ) ;
#13401 = DIRECTION ( 'NONE',  ( 0.000000000000000000, 1.000000000000000000, 0.000000000000000000 ) ) ;
#13402 = CARTESIAN_POINT ( 'NONE',  ( 44.91013252490152752, 60.79948385550241596, 3.727524721679198461 ) ) ;
#13403 = CARTESIAN_POINT ( 'NONE',  ( 45.90387839640208512, 56.30051614449765651, -5.676469297603124353 ) ) ;
#13404 = CARTESIAN_POINT ( 'NONE',  ( 52.62207051974829852, 58.60051614449766788, -7.992620115222797139 ) ) ;
#13405 = CARTESIAN_POINT ( 'NONE',  ( -4.000000000000000000, -0.8382240730041925492, -3.220610619767135141 ) ) ;
#13406 = EDGE_CURVE ( 'NONE', #3770, #12722, #11216, .T. ) ;
#13407 = CARTESIAN_POINT ( 'NONE',  ( 57.61547081786810764, 46.90051614449766504, -2.450534656007114176 ) ) ;
#13408 = COLOUR_RGB ( '',0.8941176470588234615, 0.8941176470588234615, 0.8941176470588234615 ) ;
#13410 = EDGE_LOOP ( 'NONE', ( #4767, #8729, #5874, #12755 ) ) ;
#13409 = VERTEX_POINT ( 'NONE', #5909 ) ;
#13411 = VERTEX_POINT ( 'NONE', #10108 ) ;
#13412 = UNCERTAINTY_MEASURE_WITH_UNIT (LENGTH_MEASURE( 1.000000000000000082E-05 ), #11899, 'distance_accuracy_value', 'NONE');
#13413 = ORIENTED_EDGE ( 'NONE', *, *, #11964, .T. ) ;
#13414 = EDGE_CURVE ( 'NONE', #10018, #4781, #12020, .T. ) ;
#13415 = ORIENTED_EDGE ( 'NONE', *, *, #8473, .T. ) ;
#13416 = LINE ( 'NONE', #3960, #9387 ) ;
#13417 = FACE_OUTER_BOUND ( 'NONE', #1774, .T. ) ;
#13418 = APPLICATION_CONTEXT ( 'automotive_design' ) ;
#13419 = PRODUCT_CONTEXT ( 'NONE', #1148, 'mechanical' ) ;
#13420 = CARTESIAN_POINT ( 'NONE',  ( 47.70284917648453415, 61.39948385550241738, -6.992620115222774047 ) ) ;
#13421 = AXIS2_PLACEMENT_3D ( 'NONE', #9187, #9256, #13448 ) ;
#13422 = CARTESIAN_POINT ( 'NONE',  ( 52.25172492374522903, 59.59948385550239891, -7.007379884777227730 ) ) ;
#13423 = MECHANICAL_DESIGN_GEOMETRIC_PRESENTATION_REPRESENTATION (  '', ( #10567 ), #12117 ) ;
#13424 = CARTESIAN_POINT ( 'NONE',  ( -4.000000000000000000, 2.309401076758498483, -3.433295621305379353 ) ) ;
#13425 = DIRECTION ( 'NONE',  ( 0.000000000000000000, -0.000000000000000000, 1.000000000000000000 ) ) ;
#13426 = FACE_OUTER_BOUND ( 'NONE', #406, .T. ) ;
#13427 = CARTESIAN_POINT ( 'NONE',  ( 43.33558569842706021, 47.90051614449765793, 2.141517661632167169 ) ) ;
#13428 = CARTESIAN_POINT ( 'NONE',  ( 51.92680522751233951, 51.59948385550240602, -6.007379884777223289 ) ) ;
#13429 = DIRECTION ( 'NONE',  ( 0.000000000000000000, -0.000000000000000000, 1.000000000000000000 ) ) ;
#13430 = ORIENTED_EDGE ( 'NONE', *, *, #9827, .F. ) ;
#13431 = EDGE_LOOP ( 'NONE', ( #5471, #1662, #2449, #13483 ) ) ;
#13432 = VERTEX_POINT ( 'NONE', #764 ) ;
#13433 = CARTESIAN_POINT ( 'NONE',  ( 4.170895651974849017, -2.054890354522642237, -3.559174498016357102 ) ) ;
#13434 = TOROIDAL_SURFACE ( 'NONE', #13655, 3.299999999999999822, 0.2000000000000000111 ) ;
#13435 = DIRECTION ( 'NONE',  ( -1.000000000000000000, -0.000000000000000000, -0.000000000000000000 ) ) ;
#13436 = FACE_OUTER_BOUND ( 'NONE', #1827, .T. ) ;
#13437 = DIRECTION ( 'NONE',  ( -0.000000000000000000, -0.000000000000000000, -1.000000000000000000 ) ) ;
#13438 = CARTESIAN_POINT ( 'NONE',  ( -2.725741868435985094, 3.045094352034055429, -3.220599429844047012 ) ) ;
#13439 = CARTESIAN_POINT ( 'NONE',  ( 55.71335778527780036, 46.90051614449766504, -1.832500667257213056 ) ) ;
#13440 = CARTESIAN_POINT ( 'NONE',  ( 1.498123826657866475, -5.075000000000000178, 9.000000000000000000 ) ) ;
#13441 = CARTESIAN_POINT ( 'NONE',  ( 47.70284917648453415, 57.39948385550241028, -6.992620115222774047 ) ) ;
#13442 = CARTESIAN_POINT ( 'NONE',  ( 49.97728705011488159, 53.49948385550240459, -7.000000000000000888 ) ) ;
#13443 = VERTEX_POINT ( 'NONE', #9085 ) ;
#13444 = EDGE_CURVE ( 'NONE', #13146, #1489, #8048, .T. ) ;
#13445 = CARTESIAN_POINT ( 'NONE',  ( 45.90387839640214196, 50.69948385550240744, 5.676469297603166098 ) ) ;
#13446 = ADVANCED_FACE ( 'NONE', ( #7154 ), #12881, .T. ) ;
#13447 = VERTEX_POINT ( 'NONE', #2857 ) ;
#13448 = DIRECTION ( 'NONE',  ( 0.000000000000000000, -0.5000000000000004441, 0.8660254037844383745 ) ) ;
#13449 = AXIS2_PLACEMENT_3D ( 'NONE', #9866, #10897, #1416 ) ;
#13450 = EDGE_LOOP ( 'NONE', ( #1898, #7093, #7311, #11393 ) ) ;
#13451 = EDGE_CURVE ( 'NONE', #3416, #7846, #13416, .T. ) ;
#13452 = DIRECTION ( 'NONE',  ( -0.9914448613738102711, -0.1305261922200524338, 0.000000000000000000 ) ) ;
#13453 = CARTESIAN_POINT ( 'NONE',  ( 20.00000000000000000, -14.99999999999999289, -20.00000000000000000 ) ) ;
#13454 = CARTESIAN_POINT ( 'NONE',  ( 52.25172492374522903, 47.59948385550240602, -7.007379884777227730 ) ) ;
#13455 = CARTESIAN_POINT ( 'NONE',  ( 44.91013252490150620, 58.20051614449766220, -3.727524721679154940 ) ) ;
#13456 = CARTESIAN_POINT ( 'NONE',  ( 0.1397371499201710277, 1.362866705336852169, -3.500000000000000000 ) ) ;
#13457 = CARTESIAN_POINT ( 'NONE',  ( 47.42335538002188144, 58.59948385550239891, 8.007379884777233059 ) ) ;
#13458 = COLOUR_RGB ( '',0.8941176470588234615, 0.8941176470588234615, 0.8941176470588234615 ) ;
#13459 = AXIS2_PLACEMENT_3D ( 'NONE', #7512, #11785, #2216 ) ;
#13460 = CARTESIAN_POINT ( 'NONE',  ( 3.129923130707922496, -23.63917314727666152, -8.999999999999996447 ) ) ;
#13461 = CARTESIAN_POINT ( 'NONE',  ( 57.60143344285433642, 51.89948385550241028, -2.493737253992118319 ) ) ;
#13462 = VERTEX_POINT ( 'NONE', #3131 ) ;
#13463 = ORIENTED_EDGE ( 'NONE', *, *, #8044, .F. ) ;
#13464 = ORIENTED_EDGE ( 'NONE', *, *, #6031, .T. ) ;
#13465 = DIRECTION ( 'NONE',  ( 1.000000000000000000, 0.000000000000000000, 0.000000000000000000 ) ) ;
#13466 = AXIS2_PLACEMENT_3D ( 'NONE', #10235, #5968, #1582 ) ;
#13467 = CYLINDRICAL_SURFACE ( 'NONE', #4465, 2.100000000000000089 ) ;
#13468 = DIRECTION ( 'NONE',  ( -1.000000000000000000, 0.000000000000000000, -0.000000000000000000 ) ) ;
#13469 = ADVANCED_FACE ( 'NONE', ( #219, #4437, #4307 ), #7489, .T. ) ;
#13470 = CARTESIAN_POINT ( 'NONE',  ( 2.756197834950227410, 3.027510591568626896, -3.223146290109805356 ) ) ;
#13471 = CARTESIAN_POINT ( 'NONE',  ( 55.69932041026404335, 59.89948385550240317, -1.875703265242203432 ) ) ;
#13472 = CARTESIAN_POINT ( 'NONE',  ( 52.25172492374528588, 51.40051614449767214, 7.007379884777204637 ) ) ;
#13473 = CARTESIAN_POINT ( 'NONE',  ( 43.18075615816994173, 57.80051614449766362, 4.924951120819380357 ) ) ;
#13474 = DIRECTION ( 'NONE',  ( 0.000000000000000000, 0.000000000000000000, -1.000000000000000000 ) ) ;
#13475 = B_SPLINE_CURVE_WITH_KNOTS ( 'NONE', 3,
 ( #12660, #10390, #11361, #3200, #2147, #900 ),
 .UNSPECIFIED., .F., .F.,
 ( 4, 2, 4 ),
 ( 0.000000000000000000, 0.0002095117440854740156, 0.0004190234881709480313 ),
 .UNSPECIFIED. ) ;
#13476 = CARTESIAN_POINT ( 'NONE',  ( 50.02271294988505446, 48.50051614449765935, -8.000000000000001776 ) ) ;
#13477 = AXIS2_PLACEMENT_3D ( 'NONE', #12209, #8208, #4055 ) ;
#13478 = PRODUCT ( 'hex flange nut gradea_iso_ISO - 4161 - M5 - N', 'hex flange nut gradea_iso_ISO - 4161 - M5 - N', '', ( #6061 ) ) ;
#13480 = ORIENTED_EDGE ( 'NONE', *, *, #11247, .F. ) ;
#13479 = ORIENTED_EDGE ( 'NONE', *, *, #11531, .T. ) ;
#13481 = EDGE_CURVE ( 'NONE', #9006, #2696, #6021, .T. ) ;
#13482 = ORIENTED_EDGE ( 'NONE', *, *, #8638, .F. ) ;
#13483 = ORIENTED_EDGE ( 'NONE', *, *, #1613, .F. ) ;
#13484 = DIRECTION ( 'NONE',  ( 1.000000000000000000, 0.000000000000000000, 0.000000000000000000 ) ) ;
#13485 = SURFACE_STYLE_USAGE ( .BOTH. , #11693 ) ;
#13486 = DIRECTION ( 'NONE',  ( 1.000000000000000000, 0.000000000000000000, 0.000000000000000000 ) ) ;
#13487 = DIRECTION ( 'NONE',  ( 0.000000000000000000, -0.8660254037844380415, 0.5000000000000011102 ) ) ;
#13488 = CARTESIAN_POINT ( 'NONE',  ( 55.71335778527780747, 46.09948385550240602, 1.832500667257165983 ) ) ;
#13489 = ADVANCED_FACE ( 'NONE', ( #13624, #8458 ), #82, .T. ) ;
#13490 = CARTESIAN_POINT ( 'NONE',  ( 50.02271294988512551, 58.49948385550241170, 7.000000000000000888 ) ) ;
#13491 = AXIS2_PLACEMENT_3D ( 'NONE', #3493, #5450, #2514 ) ;
#13492 = CARTESIAN_POINT ( 'NONE',  ( 1.925929944387235853E-31, 15.00000000000001599, 15.00000000000000000 ) ) ;
#13493 = FACE_OUTER_BOUND ( 'NONE', #2054, .T. ) ;
#13494 = DIRECTION ( 'NONE',  ( -1.000000000000000000, 0.000000000000000000, 0.000000000000000000 ) ) ;
#13495 = CARTESIAN_POINT ( 'NONE',  ( 57.36023556966787851, 51.00051614449763804, 0.02388180880515038476 ) ) ;
#13496 = CARTESIAN_POINT ( 'NONE',  ( 48.02776887271745210, 55.39948385550240317, -5.992620115222778487 ) ) ;
#13497 = DIRECTION ( 'NONE',  ( -0.9768494444668812671, -0.2139279384389642935, 0.000000000000000000 ) ) ;
#13498 = EDGE_LOOP ( 'NONE', ( #2452, #2381, #12155, #6602 ) ) ;
#13499 = AXIS2_PLACEMENT_3D ( 'NONE', #8442, #9800, #12648 ) ;
#13500 = LINE ( 'NONE', #842, #13366 ) ;
#13501 = VECTOR ( 'NONE', #13288, 1000.000000000000000 ) ;
#13502 = ORIENTED_EDGE ( 'NONE', *, *, #5228, .T. ) ;
#13503 = ORIENTED_EDGE ( 'NONE', *, *, #11221, .F. ) ;
#13504 = CARTESIAN_POINT ( 'NONE',  ( -7.499999999999923617, -32.99038105676662269, -9.000000000000000000 ) ) ;
#13505 = CARTESIAN_POINT ( 'NONE',  ( 6.541334219041337050, 2.934241909852039143, -5.143243597038033244 ) ) ;
#13506 = CARTESIAN_POINT ( 'NONE',  ( 6.452281807715817941, -2.898928808472988283, 5.021091983800338276 ) ) ;
#13507 = CARTESIAN_POINT ( 'NONE',  ( -2.649999999999988365, 15.00000000000001599, 15.00000000000000000 ) ) ;
#13508 = CARTESIAN_POINT ( 'NONE',  ( -74.99999999999997158, 40.00000000000001421, 15.00000000000000000 ) ) ;
#13509 = CARTESIAN_POINT ( 'NONE',  ( 3.951447005078454477, -3.704664227300105583, -0.5833333333333333703 ) ) ;
#13510 = CARTESIAN_POINT ( 'NONE',  ( 44.91013252490150620, 46.20051614449766220, -3.727524721679154940 ) ) ;
#13511 = DIRECTION ( 'NONE',  ( 0.000000000000000000, 0.000000000000000000, -1.000000000000000000 ) ) ;
#13512 = CARTESIAN_POINT ( 'NONE',  ( 55.94051828345050836, 63.79948385550240886, -4.345558710429104465 ) ) ;
#13513 = CARTESIAN_POINT ( 'NONE',  ( 52.29715082351547295, 56.39948385550238896, 6.992620115222774047 ) ) ;
#13514 = AXIS2_PLACEMENT_3D ( 'NONE', #8110, #12386, #2848 ) ;
#13515 = EDGE_CURVE ( 'NONE', #11343, #3329, #11695, .T. ) ;
#13516 = EDGE_LOOP ( 'NONE', ( #8898, #7472, #12988, #1541 ) ) ;
#13517 = CARTESIAN_POINT ( 'NONE',  ( 44.05948171654949874, 48.79948385550238754, 4.345558710429105354 ) ) ;
#13518 = AXIS2_PLACEMENT_3D ( 'NONE', #10319, #825, #13484 ) ;
#13519 = EDGE_LOOP ( 'NONE', ( #12120, #12453, #8042, #10165 ) ) ;
#13520 = CARTESIAN_POINT ( 'NONE',  ( 4.030875481282487627, 1.403567514399325367, 3.500000000000000000 ) ) ;
#13521 = ORIENTED_EDGE ( 'NONE', *, *, #5683, .F. ) ;
#13522 = EDGE_CURVE ( 'NONE', #10854, #10505, #2218, .T. ) ;
#13523 = DIRECTION ( 'NONE',  ( 1.000000000000000000, 0.000000000000000000, 0.000000000000000000 ) ) ;
#13524 = AXIS2_PLACEMENT_3D ( 'NONE', #11477, #10438, #2832 ) ;
#13525 = DIRECTION ( 'NONE',  ( -4.082155997157844188E-16, 1.000000000000000000, 0.000000000000000000 ) ) ;
#13526 = CARTESIAN_POINT ( 'NONE',  ( 44.05948171654949874, 48.79948385550239465, 4.345558710429104465 ) ) ;
#13527 = EDGE_CURVE ( 'NONE', #11879, #3807, #12662, .T. ) ;
#13528 = CARTESIAN_POINT ( 'NONE',  ( 42.63976443033212860, 50.00051614449766646, -0.02388180880514948964 ) ) ;
#13529 = EDGE_CURVE ( 'NONE', #9438, #11340, #6462, .T. ) ;
#13530 = FACE_OUTER_BOUND ( 'NONE', #12391, .T. ) ;
#13531 = CARTESIAN_POINT ( 'NONE',  ( 42.39856655714566358, 60.89948385550241028, 2.493737253992119207 ) ) ;
#13532 =( GEOMETRIC_REPRESENTATION_CONTEXT ( 3 ) GLOBAL_UNCERTAINTY_ASSIGNED_CONTEXT ( ( #5009 ) ) GLOBAL_UNIT_ASSIGNED_CONTEXT ( ( #9177, #12485, #13371 ) ) REPRESENTATION_CONTEXT ( 'NONE', 'WORKASPACE' ) );
#13533 = CARTESIAN_POINT ( 'NONE',  ( 2.499999999999999556, 0.000000000000000000, 3.469446951953614189E-15 ) ) ;
#13534 = CARTESIAN_POINT ( 'NONE',  ( -4.211140560182196957, -2.431303136016552013, -3.745885042887436178 ) ) ;
#13535 = EDGE_CURVE ( 'NONE', #5152, #2821, #958, .T. ) ;
#13536 = CARTESIAN_POINT ( 'NONE',  ( 54.72065718078924590, 48.29948385550240175, 6.458785618021043895 ) ) ;
#13537 = VERTEX_POINT ( 'NONE', #5225 ) ;
#13538 = ORIENTED_EDGE ( 'NONE', *, *, #12917, .F. ) ;
#13539 = ORIENTED_EDGE ( 'NONE', *, *, #2896, .F. ) ;
#13540 = DIRECTION ( 'NONE',  ( -1.000000000000000000, 0.000000000000000000, -0.000000000000000000 ) ) ;
#13541 =( NAMED_UNIT ( * ) SI_UNIT ( $, .STERADIAN. ) SOLID_ANGLE_UNIT ( ) );
#13542 = DIRECTION ( 'NONE',  ( 0.000000000000000000, 0.000000000000000000, 1.000000000000000000 ) ) ;
#13543 = CARTESIAN_POINT ( 'NONE',  ( 6.390983399715589819, -2.822795037344614233, 5.110775575965824657 ) ) ;
#13544 = CARTESIAN_POINT ( 'NONE',  ( 3.540020015735602765, 2.810662092924382627, -3.602146406945867962 ) ) ;
#13545 = CARTESIAN_POINT ( 'NONE',  ( 51.97223112728254790, 62.39948385550240317, 5.992620115222778487 ) ) ;
#13546 = CARTESIAN_POINT ( 'NONE',  ( 42.63976443033212149, 60.00051614449765225, -0.02388180880514948964 ) ) ;
#13547 = VECTOR ( 'NONE', #9311, 1000.000000000000000 ) ;
#13548 = CARTESIAN_POINT ( 'NONE',  ( 56.79116909180259398, 57.20051614449766220, 4.963592699178938972 ) ) ;
#13549 = CARTESIAN_POINT ( 'NONE',  ( 4.000000000000000000, 0.9868501483902631932, -0.09357334158579604100 ) ) ;
#13550 = CONICAL_SURFACE ( 'NONE', #1624, 1.999999999999998224, 1.029744259999999745 ) ;
#13551 = CARTESIAN_POINT ( 'NONE',  ( 43.20883090819742023, 50.20051614449766220, -4.963592699178938972 ) ) ;
#13552 = CIRCLE ( 'NONE', #11129, 2.000000000000001332 ) ;
#13554 = VERTEX_POINT ( 'NONE', #9427 ) ;
#13553 = ORIENTED_EDGE ( 'NONE', *, *, #5638, .T. ) ;
#13555 = ORIENTED_EDGE ( 'NONE', *, *, #533, .F. ) ;
#13556 = ORIENTED_EDGE ( 'NONE', *, *, #488, .T. ) ;
#13557 = AXIS2_PLACEMENT_3D ( 'NONE', #8663, #12860, #10459 ) ;
#13558 = CARTESIAN_POINT ( 'NONE',  ( 6.466260427357665819, 5.808561367196023895, -1.902591328531564046E-16 ) ) ;
#13559 = CARTESIAN_POINT ( 'NONE',  ( -1.000000000000000000, -14.00000000000000000, -9.000000000000001776 ) ) ;
#13560 = DIRECTION ( 'NONE',  ( -0.000000000000000000, 0.000000000000000000, 1.000000000000000000 ) ) ;
#13561 = VECTOR ( 'NONE', #4757, 1000.000000000000000 ) ;
#13562 = DIRECTION ( 'NONE',  ( 0.000000000000000000, -0.000000000000000000, 1.000000000000000000 ) ) ;
#13563 = CARTESIAN_POINT ( 'NONE',  ( 57.36023556966787851, 61.99948385550241170, -0.02388180880522424582 ) ) ;
#13564 = EDGE_CURVE ( 'NONE', #2067, #1223, #6726, .T. ) ;
#13565 = CARTESIAN_POINT ( 'NONE',  ( 55.96859303347805081, 60.19948385550240033, 4.306917132069425058 ) ) ;
#13566 = CARTESIAN_POINT ( 'NONE',  ( 47.74827507625469281, 60.40051614449767214, -7.007379884777203749 ) ) ;
#13567 = DIRECTION ( 'NONE',  ( 0.8191520442889902442, 1.003171929053522651E-16, -0.5735764363510482688 ) ) ;
#13568 = CIRCLE ( 'NONE', #108, 4.800000000000000711 ) ;
#13569 = CARTESIAN_POINT ( 'NONE',  ( 17.85000000000000142, -20.00000000000000000, -20.00000000000000000 ) ) ;
#13570 = CARTESIAN_POINT ( 'NONE',  ( -4.211140560182196957, 2.431303136016537803, -3.745885042887433514 ) ) ;
#13571 = CARTESIAN_POINT ( 'NONE',  ( 55.94051828345053679, 51.20051614449766220, 4.345558710429044069 ) ) ;
#13572 = CARTESIAN_POINT ( 'NONE',  ( 55.69932041026404335, 51.89948385550241028, -1.875703265242203432 ) ) ;
#13573 = CARTESIAN_POINT ( 'NONE',  ( 0.000000000000000000, 4.330127018922190985, 2.500000000000005329 ) ) ;
#13574 = VERTEX_POINT ( 'NONE', #10664 ) ;
#13575 = CARTESIAN_POINT ( 'NONE',  ( 5.000000000000003553, -20.00000000000000000, 15.00000000000000355 ) ) ;
#13576 = VERTEX_POINT ( 'NONE', #7428 ) ;
#13577 = ORIENTED_EDGE ( 'NONE', *, *, #11527, .T. ) ;
#13578 = CARTESIAN_POINT ( 'NONE',  ( 0.6666666666666689611, 4.233901974057261874, -3.300726591567082480 ) ) ;
#13579 = CARTESIAN_POINT ( 'NONE',  ( 6.390820841722129941, 5.837016270311235822, 0.1100087447852453187 ) ) ;
#13580 = CARTESIAN_POINT ( 'NONE',  ( 6.390820551024316565, -3.013776919160863876, 4.999999999999999112 ) ) ;
#13581 =( NAMED_UNIT ( * ) PLANE_ANGLE_UNIT ( ) SI_UNIT ( $, .RADIAN. ) );
#13582 = CARTESIAN_POINT ( 'NONE',  ( 57.36023556966787851, 45.99948385550238328, -0.02388180880522424582 ) ) ;
#13583 = FACE_OUTER_BOUND ( 'NONE', #7537, .T. ) ;
#13584 = CARTESIAN_POINT ( 'NONE',  ( 56.30877334542961421, 53.00051614449765935, 0.02388180880515774693 ) ) ;
#13585 = DIRECTION ( 'NONE',  ( 0.000000000000000000, 0.000000000000000000, 1.000000000000000000 ) ) ;
#13586 = CARTESIAN_POINT ( 'NONE',  ( 3.999999999999999112, -0.7890432684750902093, -0.04868663549882291247 ) ) ;
#13587 = CARTESIAN_POINT ( 'NONE',  ( 54.13287192849676188, 54.29948385550240886, 5.649768623646098220 ) ) ;
#13588 = EDGE_CURVE ( 'NONE', #5565, #10506, #4171, .T. ) ;
#13589 = ORIENTED_EDGE ( 'NONE', *, *, #99, .T. ) ;
#13590 = CARTESIAN_POINT ( 'NONE',  ( 43.33558569842703179, 53.09948385550240602, -2.141517661632099223 ) ) ;
#13591 = ORIENTED_EDGE ( 'NONE', *, *, #134, .F. ) ;
#13592 = CARTESIAN_POINT ( 'NONE',  ( 3.974183935050568106, -0.7239581970520293508, 3.565826011443134824 ) ) ;
#13593 = ADVANCED_FACE ( 'NONE', ( #152 ), #4507, .F. ) ;
#13594 = DIRECTION ( 'NONE',  ( -1.000000000000000000, 0.000000000000000000, 0.000000000000000000 ) ) ;
#13595 = CARTESIAN_POINT ( 'NONE',  ( 4.175813232069146785, -2.061359961916366057, 3.570380186727398542 ) ) ;
#13596 = CARTESIAN_POINT ( 'NONE',  ( -74.99999999999997158, -39.99999999999998579, 10.00000000000000000 ) ) ;
#13597 = AXIS2_PLACEMENT_3D ( 'NONE', #772, #980, #2864 ) ;
#13598 = CARTESIAN_POINT ( 'NONE',  ( 57.36023556966787851, 49.00051614449763804, 0.02388180880515038476 ) ) ;
#13599 = PRODUCT ( 'spring', 'spring', '', ( #2859 ) ) ;
#13600 = CARTESIAN_POINT ( 'NONE',  ( 6.355827204229362870, -5.411702751981846582, 0.8440485055075620524 ) ) ;
#13601 = CARTESIAN_POINT ( 'NONE',  ( 57.60143344285433642, 63.89948385550240317, -2.493737253992118319 ) ) ;
#13602 = VECTOR ( 'NONE', #11414, 1000.000000000000000 ) ;
#13603 = DIRECTION ( 'NONE',  ( -1.000000000000000000, 0.000000000000000000, 0.000000000000000000 ) ) ;
#13604 = ADVANCED_FACE ( 'NONE', ( #1037 ), #736, .T. ) ;
#13605 = CARTESIAN_POINT ( 'NONE',  ( 54.68390685589033495, 53.69948385550240744, -6.485486291978119766 ) ) ;
#13606 = EDGE_CURVE ( 'NONE', #7673, #6987, #10249, .T. ) ;
#13607 = EDGE_LOOP ( 'NONE', ( #12891, #11211 ) ) ;
#13608 = EDGE_CURVE ( 'NONE', #579, #1369, #7524, .T. ) ;
#13609 = ORIENTED_EDGE ( 'NONE', *, *, #7519, .F. ) ;
#13610 = CARTESIAN_POINT ( 'NONE',  ( 54.23491683972284960, 45.00000000000001421, -4.999999999999999112 ) ) ;
#13611 = LINE ( 'NONE', #5272, #8226 ) ;
#13612 = DIRECTION ( 'NONE',  ( -0.000000000000000000, -0.000000000000000000, 1.000000000000000000 ) ) ;
#13613 = DIRECTION ( 'NONE',  ( 0.000000000000000000, 0.000000000000000000, -1.000000000000000000 ) ) ;
#13614 = CARTESIAN_POINT ( 'NONE',  ( 53.54508667620424234, 48.70051614449766930, -4.840751629271188961 ) ) ;
#13615 = CARTESIAN_POINT ( 'NONE',  ( 56.66441430157294690, 62.90051614449765083, -2.141517661632166281 ) ) ;
#13616 = CARTESIAN_POINT ( 'NONE',  ( 52.62207051974839089, 46.39948385550240317, 7.992620115222770494 ) ) ;
#13617 = CARTESIAN_POINT ( 'NONE',  ( -4.211399284164270895, 2.459729995988205964, -3.751162237960538715 ) ) ;
#13618 = CARTESIAN_POINT ( 'NONE',  ( 43.20883090819742023, 48.20051614449766930, -4.963592699178938972 ) ) ;
#13619 = VERTEX_POINT ( 'NONE', #10597 ) ;
#13620 = ORIENTED_EDGE ( 'NONE', *, *, #2118, .T. ) ;
#13621 = ORIENTED_EDGE ( 'NONE', *, *, #910, .T. ) ;
#13622 = CARTESIAN_POINT ( 'NONE',  ( 10.00000000000000000, 25.00000000000001776, 15.00000000000000000 ) ) ;
#13623 = CARTESIAN_POINT ( 'NONE',  ( 5.384454397937118664, 0.000000000000000000, -5.000000000000000000 ) ) ;
#13624 = FACE_OUTER_BOUND ( 'NONE', #9794, .T. ) ;
#13625 = DIRECTION ( 'NONE',  ( 0.000000000000000000, 0.000000000000000000, 1.000000000000000000 ) ) ;
#13626 = CARTESIAN_POINT ( 'NONE',  ( 53.50833635130540955, 49.69948385550240744, -4.867452303228209765 ) ) ;
#13627 = CARTESIAN_POINT ( 'NONE',  ( 47.70284917648453415, 63.39948385550239607, -6.992620115222774047 ) ) ;
#13628 = CARTESIAN_POINT ( 'NONE',  ( 47.70284917648459100, 61.60051614449764656, 6.992620115222796251 ) ) ;
#13629=STYLED_ITEM('',(#13684),#10159);
#13630 = CARTESIAN_POINT ( 'NONE',  ( 4.175813232069148562, 4.122719923832741884, -2.765695189283172261E-17 ) ) ;
#13631 = LINE ( 'NONE', #5090, #11177 ) ;
#13632 = CARTESIAN_POINT ( 'NONE',  ( 4.180231891692620216, 4.134807952925572572, 0.02076457676760539231 ) ) ;
#13633 = CARTESIAN_POINT ( 'NONE',  ( 55.96859303347802239, 52.80051614449764941, -4.306917132069484566 ) ) ;
#13634 = CARTESIAN_POINT ( 'NONE',  ( 53.54508667620428497, 56.29948385550240886, 4.840751629271157874 ) ) ;
#13635 = FACE_OUTER_BOUND ( 'NONE', #7549, .T. ) ;
#13636 = ORIENTED_EDGE ( 'NONE', *, *, #4219, .F. ) ;
#13637 = EDGE_CURVE ( 'NONE', #966, #686, #3268, .T. ) ;
#13638 = LINE ( 'NONE', #12406, #2115 ) ;
#13639 = ORIENTED_EDGE ( 'NONE', *, *, #9304, .T. ) ;
#13640 = DIRECTION ( 'NONE',  ( -1.000000000000000000, -3.469446951953615175E-16, 0.000000000000000000 ) ) ;
#13641 = AXIS2_PLACEMENT_3D ( 'NONE', #1631, #3520, #12156 ) ;
#13642 = DIRECTION ( 'NONE',  ( 1.000000000000000000, 0.000000000000000000, -0.000000000000000000 ) ) ;
#13643 = CARTESIAN_POINT ( 'NONE',  ( 2.482347295856823136E-15, -20.00000000000000000, -8.999999999999996447 ) ) ;
#13644 = COLOUR_RGB ( '',0.8941176470588234615, 0.8941176470588234615, 0.8941176470588234615 ) ;
#13645 = CARTESIAN_POINT ( 'NONE',  ( 43.34962307344081012, 52.89948385550240317, 2.184720259617164650 ) ) ;
#13646 = CYLINDRICAL_SURFACE ( 'NONE', #3315, 15.00000000000000000 ) ;
#13647 = CARTESIAN_POINT ( 'NONE',  ( 44.88205777487401349, 49.80051614449765651, 3.688883143319584779 ) ) ;
#13648 = CARTESIAN_POINT ( 'NONE',  ( 3.098410542199072637, -7.060458129626440815, -1.000000000000000000 ) ) ;
#13649 = B_SPLINE_CURVE_WITH_KNOTS ( 'NONE', 3,
 ( #3472, #11900, #5761, #5552, #9832, #285 ),
 .UNSPECIFIED., .F., .F.,
 ( 4, 2, 4 ),
 ( 0.008261945092156346496, 0.009724140865920691962, 0.01118633663968503569 ),
 .UNSPECIFIED. ) ;
#13650 = DIRECTION ( 'NONE',  ( 1.000000000000000000, 0.000000000000000000, 0.000000000000000000 ) ) ;
#13651 = CARTESIAN_POINT ( 'NONE',  ( 45.90387839640214196, 62.69948385550240744, 5.676469297603166098 ) ) ;
#13652 = CARTESIAN_POINT ( 'NONE',  ( 54.13287192849676188, 62.29948385550240886, 5.649768623646098220 ) ) ;
#13653 = AXIS2_PLACEMENT_3D ( 'NONE', #12512, #8375, #13397 ) ;
#13654 = ORIENTED_EDGE ( 'NONE', *, *, #3208, .T. ) ;
#13655 = AXIS2_PLACEMENT_3D ( 'NONE', #9979, #701, #8060 ) ;
#13656 = ORIENTED_EDGE ( 'NONE', *, *, #10484, .F. ) ;
#13657 = CARTESIAN_POINT ( 'NONE',  ( 4.151274195509680354, 4.079825909417489349, 1.184320329358001550E-15 ) ) ;
#13658 = DIRECTION ( 'NONE',  ( -0.4999999999999924505, -0.8660254037844429265, 0.000000000000000000 ) ) ;
#13659 = DIRECTION ( 'NONE',  ( -1.000000000000000000, -0.000000000000000000, -0.000000000000000000 ) ) ;
#13660 = DIRECTION ( 'NONE',  ( -1.000000000000000000, 0.000000000000000000, 1.224646799147353207E-16 ) ) ;
#13661 = CARTESIAN_POINT ( 'NONE',  ( 45.90387839640214196, 48.69948385550240744, 5.676469297603166098 ) ) ;
#13662 = AXIS2_PLACEMENT_3D ( 'NONE', #7402, #7467, #3035 ) ;
#13663 = NEXT_ASSEMBLY_USAGE_OCCURRENCE ( 'NAUO1', ' ', ' ', #12904, #4727, $ ) ;
#13664 = NEXT_ASSEMBLY_USAGE_OCCURRENCE ( 'NAUO2', ' ', ' ', #12904, #9454, $ ) ;
#13665 = NEXT_ASSEMBLY_USAGE_OCCURRENCE ( 'NAUO3', ' ', ' ', #12904, #10465, $ ) ;
#13666 = NEXT_ASSEMBLY_USAGE_OCCURRENCE ( 'NAUO4', ' ', ' ', #12904, #10036, $ ) ;
#13667 = NEXT_ASSEMBLY_USAGE_OCCURRENCE ( 'NAUO5', ' ', ' ', #12904, #12493, $ ) ;
#13668 = NEXT_ASSEMBLY_USAGE_OCCURRENCE ( 'NAUO6', ' ', ' ', #12904, #10642, $ ) ;
#13669 = NEXT_ASSEMBLY_USAGE_OCCURRENCE ( 'NAUO7', ' ', ' ', #12904, #12073, $ ) ;
#13670 = NEXT_ASSEMBLY_USAGE_OCCURRENCE ( 'NAUO8', ' ', ' ', #12904, #12073, $ ) ;
#13671 = NEXT_ASSEMBLY_USAGE_OCCURRENCE ( 'NAUO9', ' ', ' ', #12904, #6587, $ ) ;
#13672 = NEXT_ASSEMBLY_USAGE_OCCURRENCE ( 'NAUO10', ' ', ' ', #12904, #11897, $ ) ;
#13673 = NEXT_ASSEMBLY_USAGE_OCCURRENCE ( 'NAUO11', ' ', ' ', #12904, #11897, $ ) ;
#13674 = NEXT_ASSEMBLY_USAGE_OCCURRENCE ( 'NAUO12', ' ', ' ', #12904, #11484, $ ) ;
#13675 = NEXT_ASSEMBLY_USAGE_OCCURRENCE ( 'NAUO13', ' ', ' ', #12904, #11484, $ ) ;
#13676 = NEXT_ASSEMBLY_USAGE_OCCURRENCE ( 'NAUO14', ' ', ' ', #12904, #12316, $ ) ;
#13677 = NEXT_ASSEMBLY_USAGE_OCCURRENCE ( 'NAUO15', ' ', ' ', #12904, #12316, $ ) ;
#13678=COLOUR_RGB('Dark Blue',0.08,0.2,0.34);
#13679=FILL_AREA_STYLE_COLOUR('',#13678);
#13680=FILL_AREA_STYLE('',(#13679));
#13681=SURFACE_STYLE_FILL_AREA(#13680);
#13682=SURFACE_SIDE_STYLE('',(#13681));
#13683=SURFACE_STYLE_USAGE(.BOTH.,#13682);
#13684=PRESENTATION_STYLE_ASSIGNMENT((#13683));
#13685=COLOUR_RGB('Light Blue',0.38,0.62,0.78);
#13686=FILL_AREA_STYLE_COLOUR('',#13685);
#13687=FILL_AREA_STYLE('',(#13686));
#13688=SURFACE_STYLE_FILL_AREA(#13687);
#13689=SURFACE_SIDE_STYLE('',(#13688));
#13690=SURFACE_STYLE_USAGE(.BOTH.,#13689);
#13691=PRESENTATION_STYLE_ASSIGNMENT((#13690));
#13692=COLOUR_RGB('Sky Blue',0.24,0.69,0.87);
#13693=FILL_AREA_STYLE_COLOUR('',#13692);
#13694=FILL_AREA_STYLE('',(#13693));
#13695=SURFACE_STYLE_FILL_AREA(#13694);
#13696=SURFACE_SIDE_STYLE('',(#13695));
#13697=SURFACE_STYLE_USAGE(.BOTH.,#13696);
#13698=PRESENTATION_STYLE_ASSIGNMENT((#13697));
#13699=COLOUR_RGB('Grey',0.48,0.52,0.57);
#13700=FILL_AREA_STYLE_COLOUR('',#13699);
#13701=FILL_AREA_STYLE('',(#13700));
#13702=SURFACE_STYLE_FILL_AREA(#13701);
#13703=SURFACE_SIDE_STYLE('',(#13702));
#13704=SURFACE_STYLE_USAGE(.BOTH.,#13703);
#13705=PRESENTATION_STYLE_ASSIGNMENT((#13704));
#13706=COLOUR_RGB('Black',0.12,0.14,0.17);
#13707=FILL_AREA_STYLE_COLOUR('',#13706);
#13708=FILL_AREA_STYLE('',(#13707));
#13709=SURFACE_STYLE_FILL_AREA(#13708);
#13710=SURFACE_SIDE_STYLE('',(#13709));
#13711=SURFACE_STYLE_USAGE(.BOTH.,#13710);
#13712=PRESENTATION_STYLE_ASSIGNMENT((#13711));
#13713=COLOUR_RGB('Off White',0.89,0.88,0.83);
#13714=FILL_AREA_STYLE_COLOUR('',#13713);
#13715=FILL_AREA_STYLE('',(#13714));
#13716=SURFACE_STYLE_FILL_AREA(#13715);
#13717=SURFACE_SIDE_STYLE('',(#13716));
#13718=SURFACE_STYLE_USAGE(.BOTH.,#13717);
#13719=PRESENTATION_STYLE_ASSIGNMENT((#13718));
ENDSEC;
END-ISO-10303-21;
